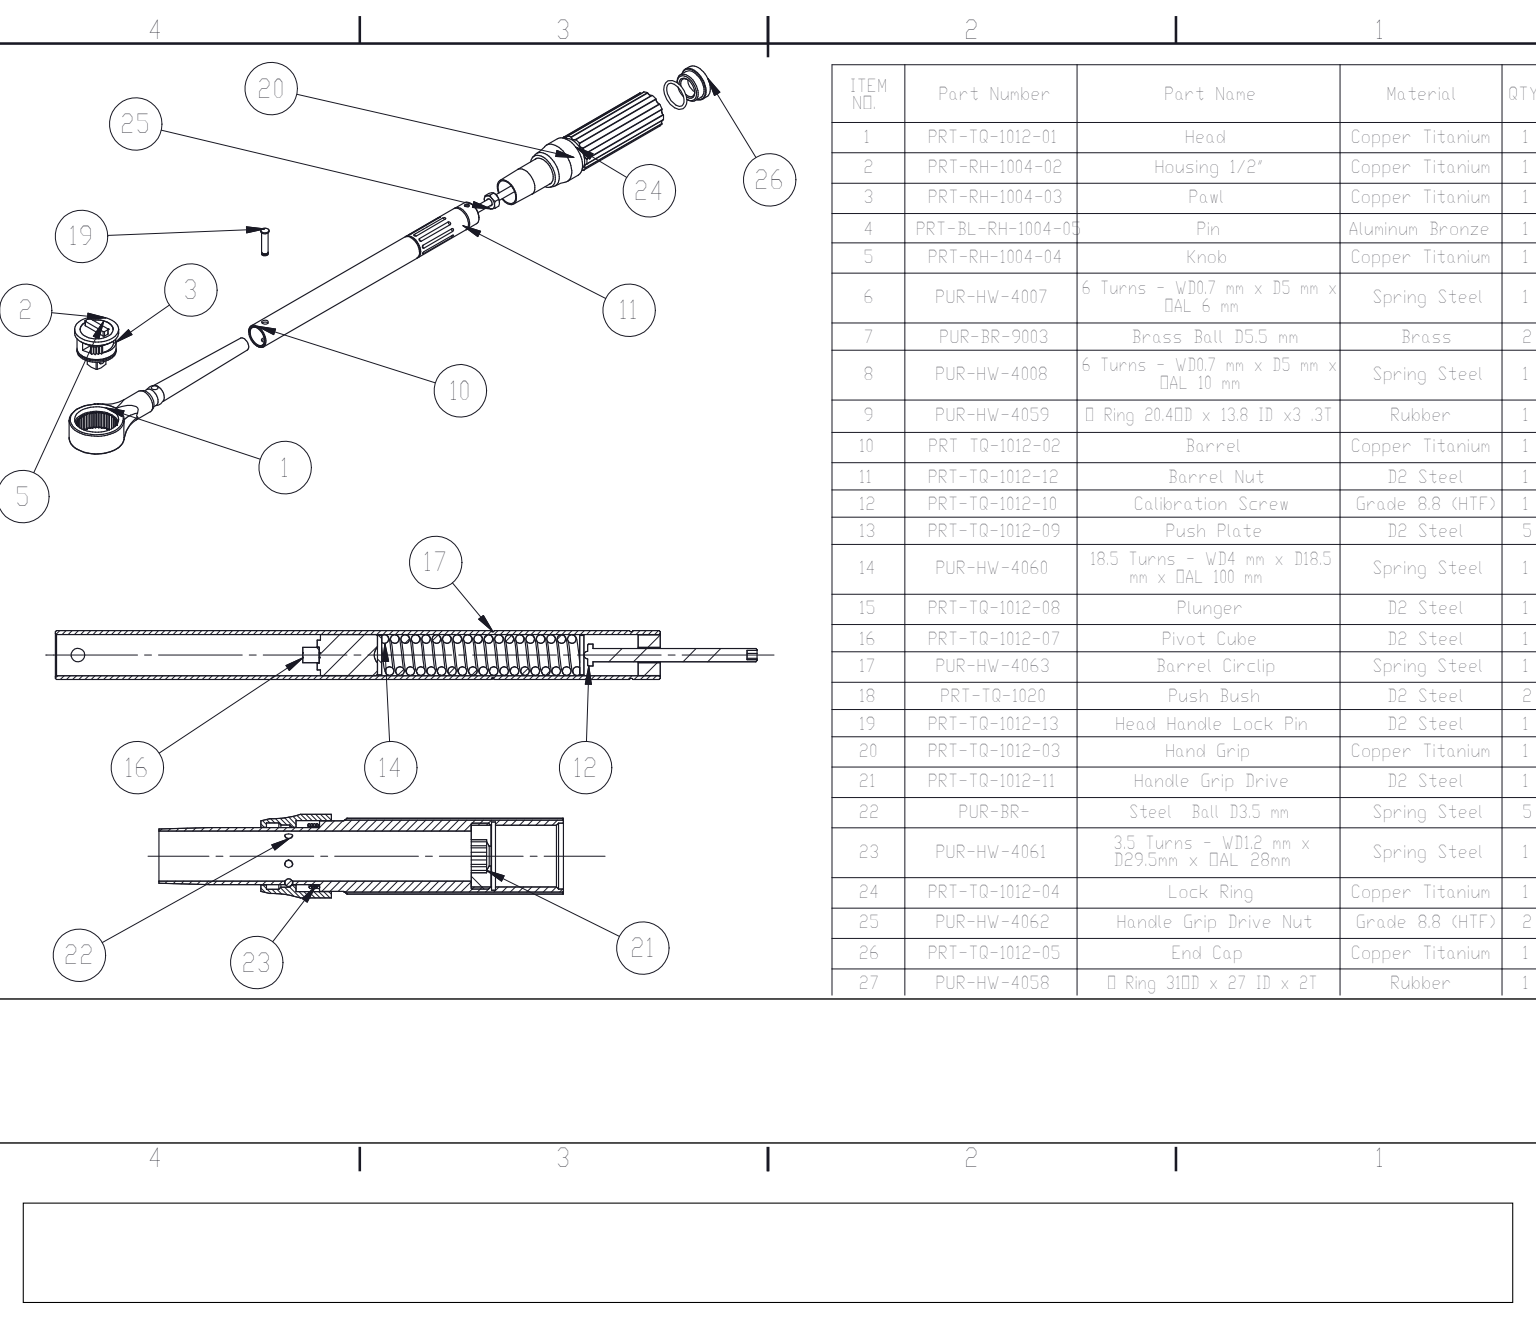
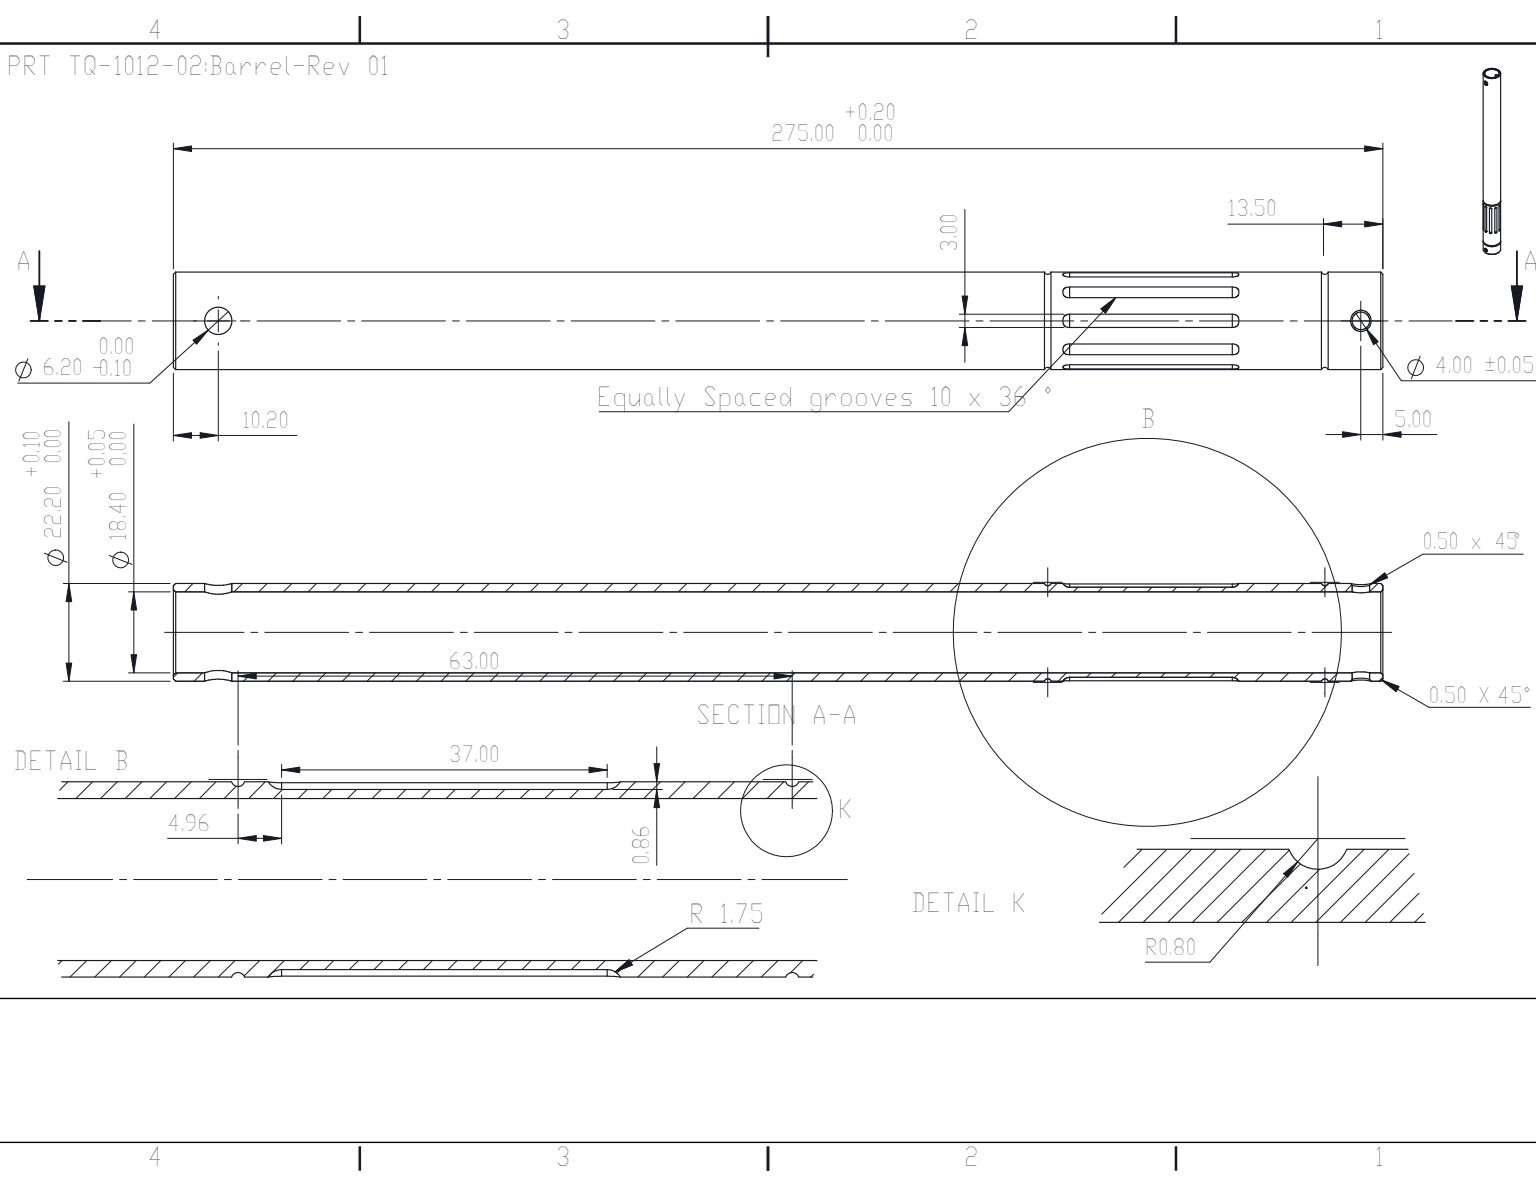
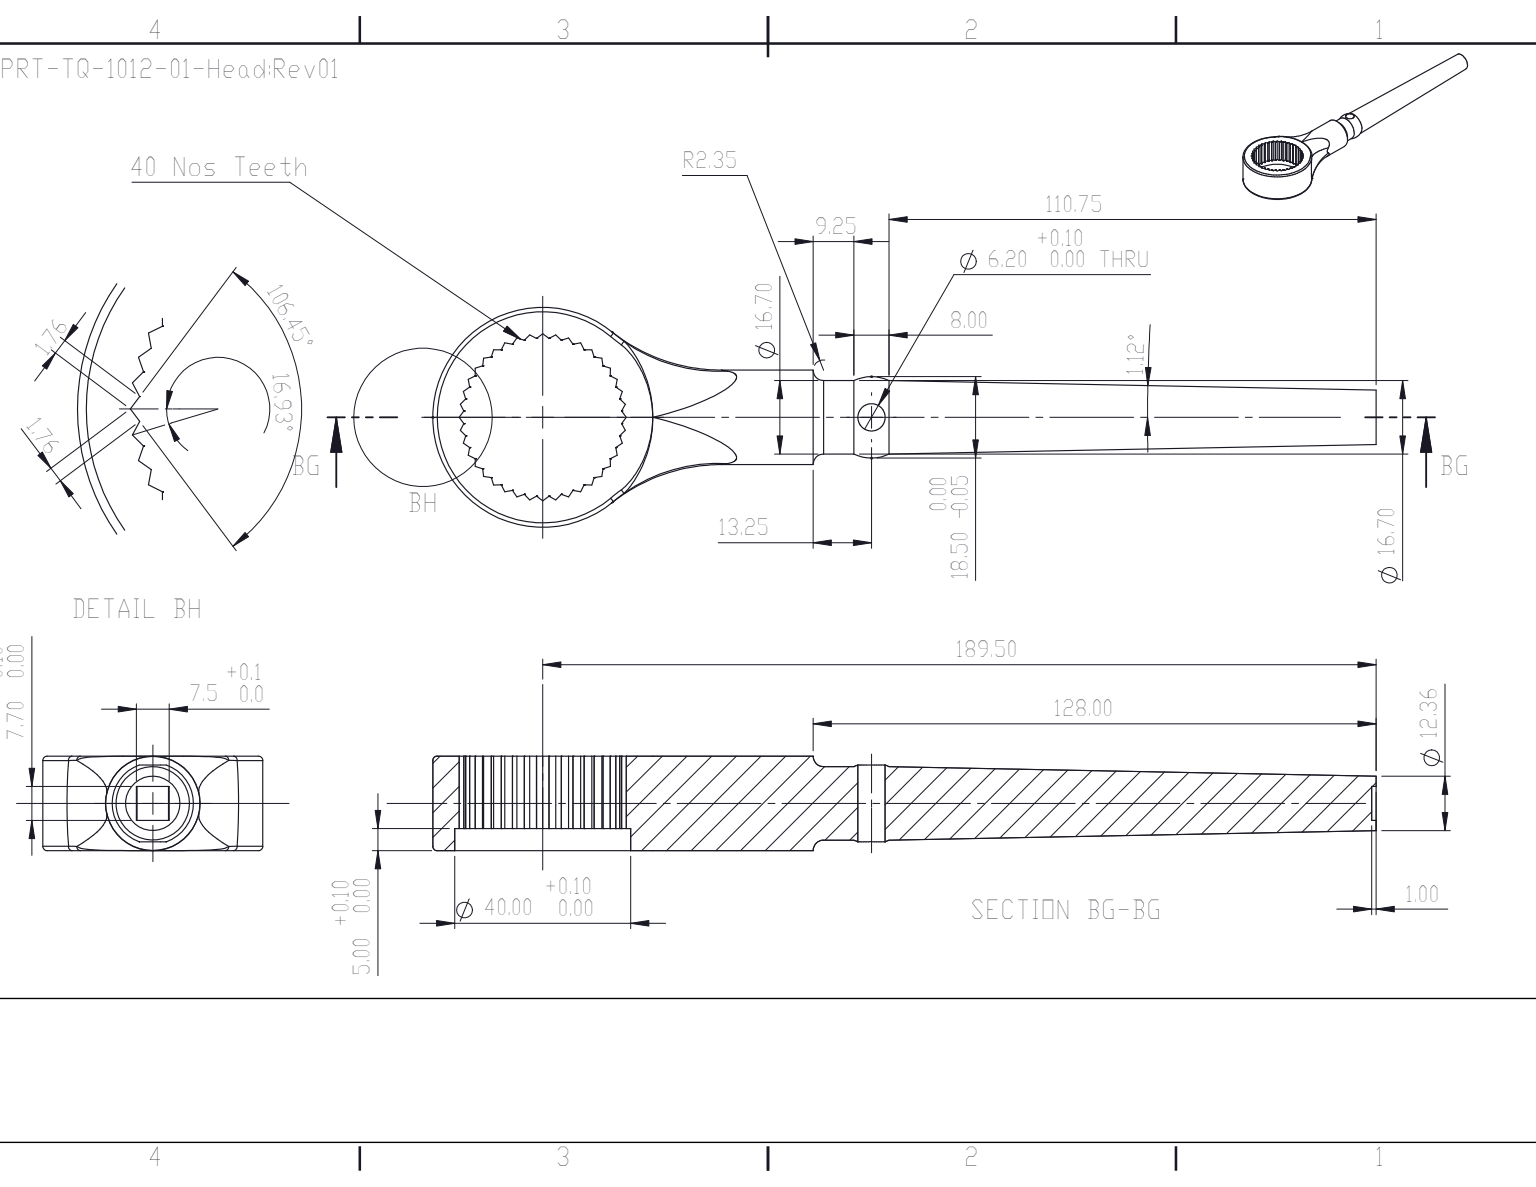
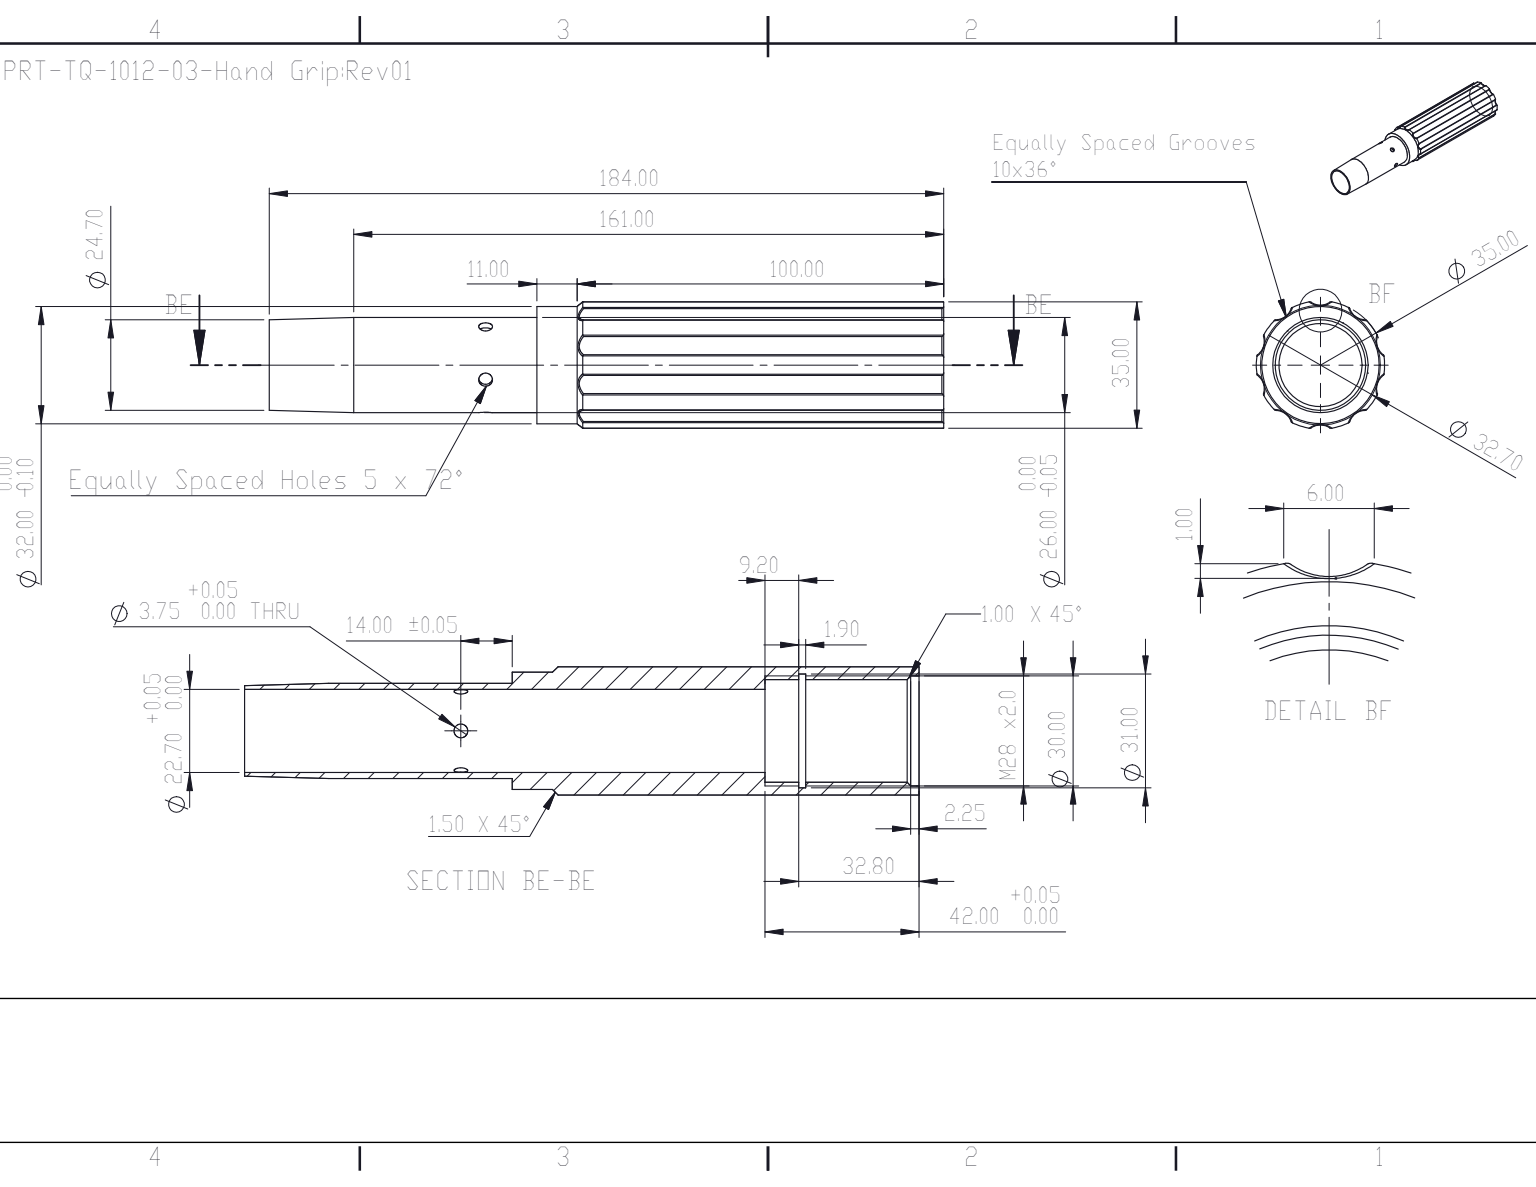
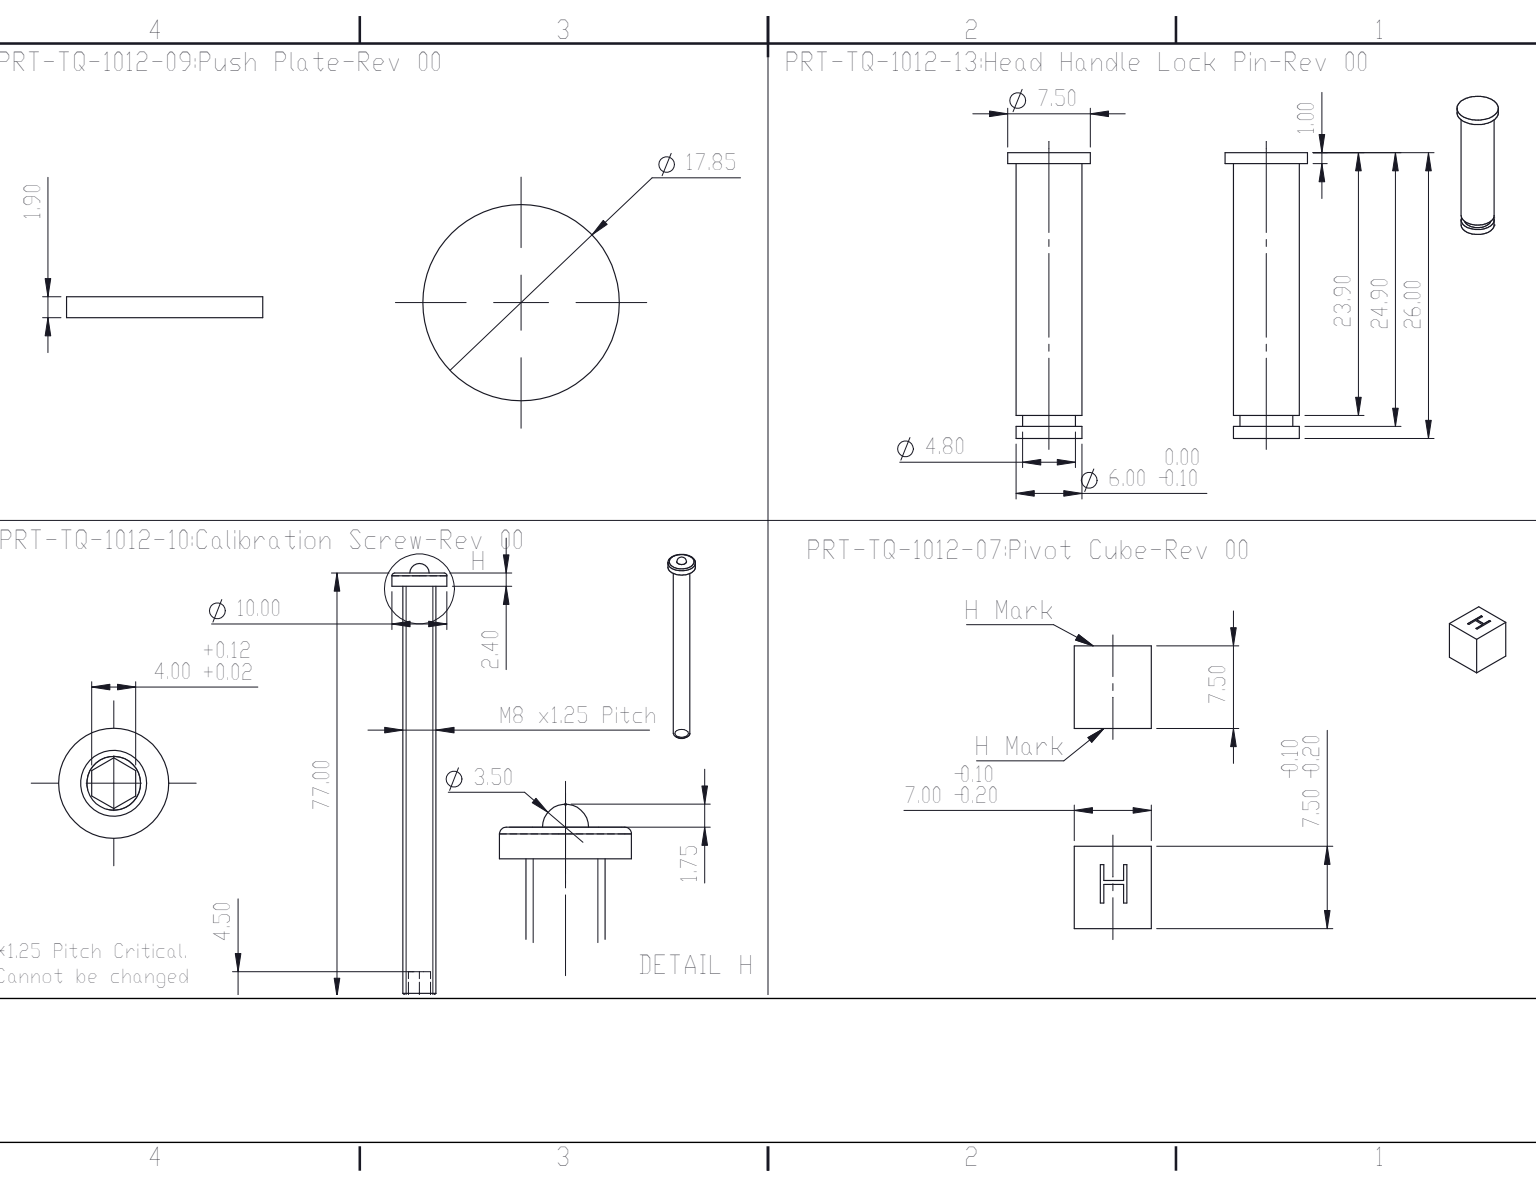
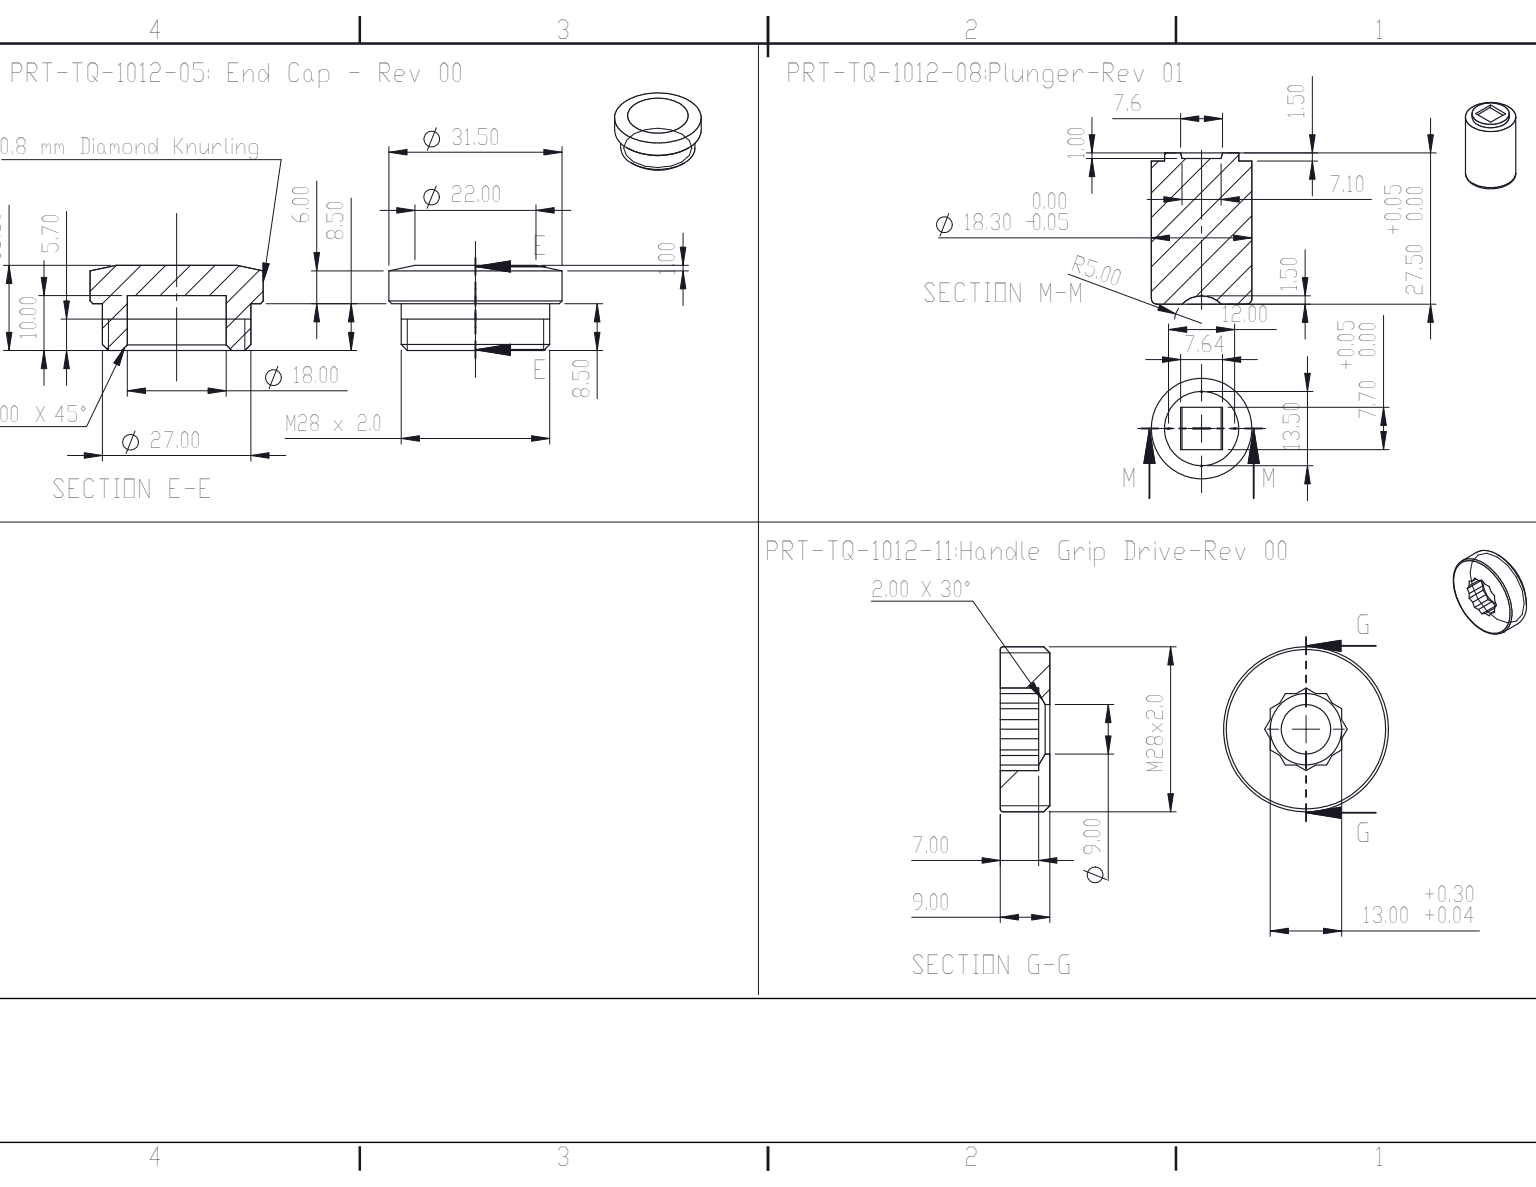
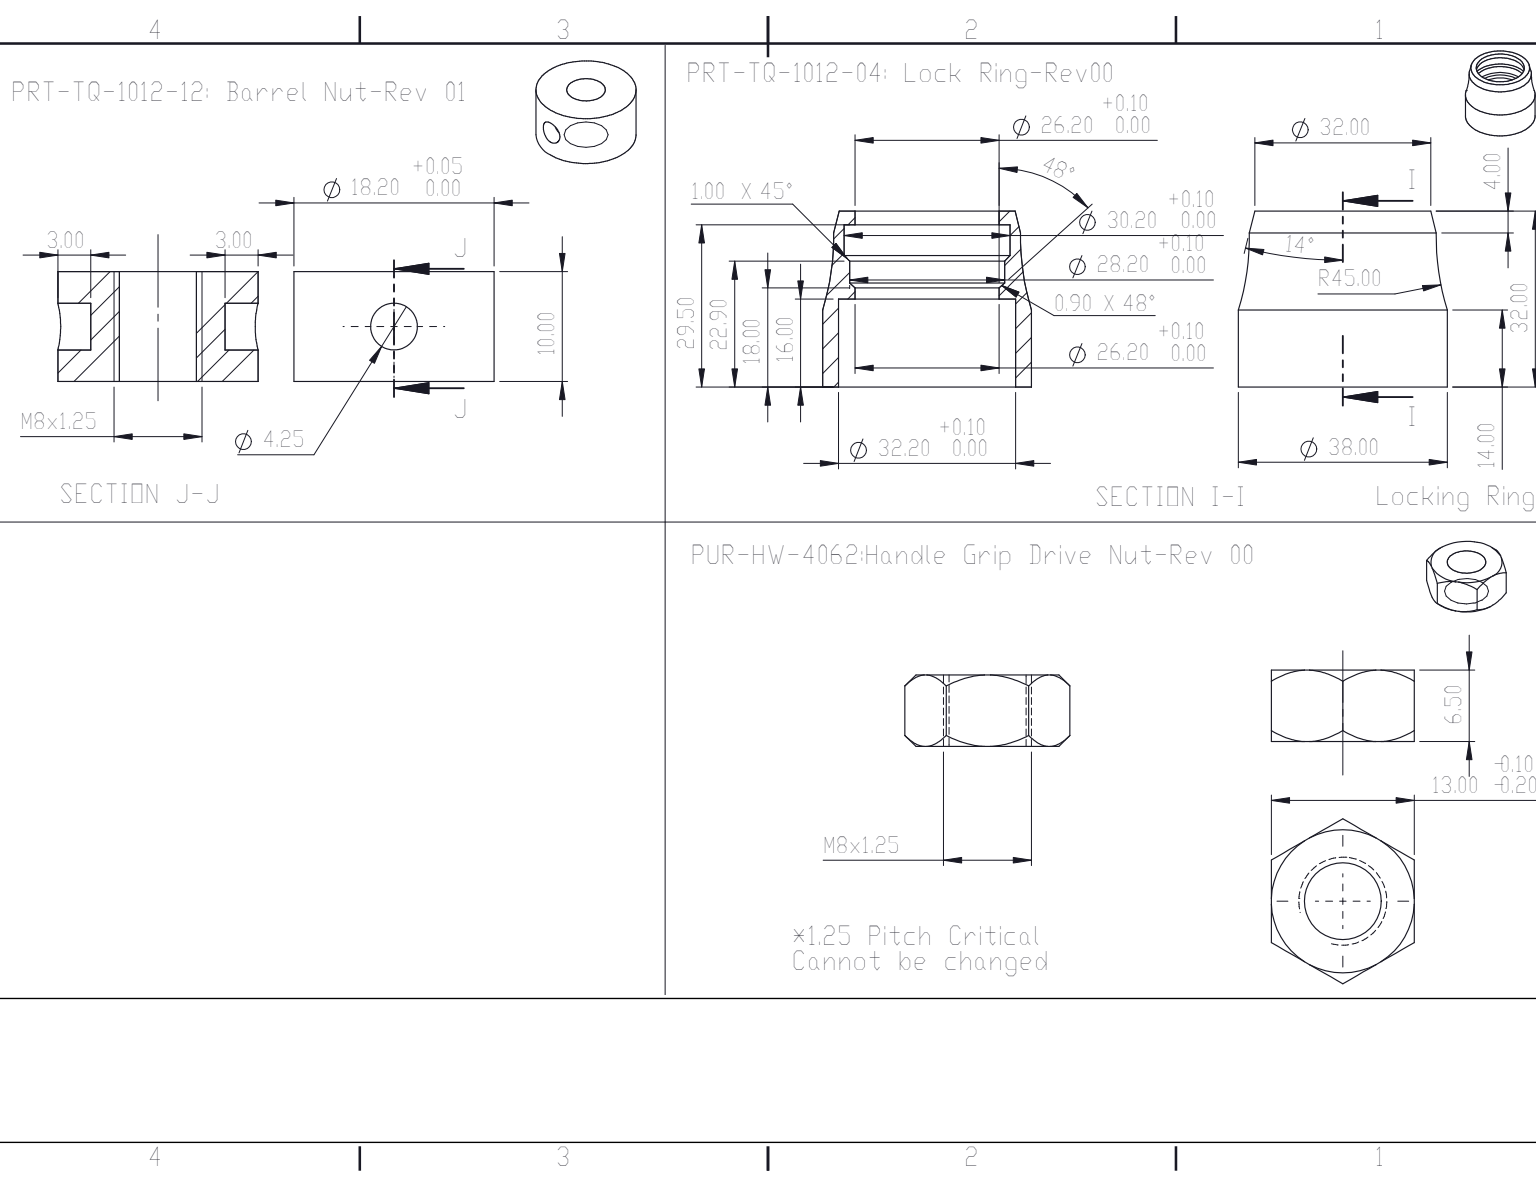
ISO-10303-21;
HEADER;
/* Generated by software containing ST-Developer
 * from STEP Tools, Inc. (www.steptools.com) 
 */

FILE_DESCRIPTION(
/* description */ ('STEP AP214'),
/* implementation_level */ '2;1');

FILE_NAME(
/* name */ 'MAS-618',
/* time_stamp */ '2026-10-07T12:49:37-07:00',
/* author */ (''),
/* organization */ (''),
/* preprocessor_version */ 'ST-DEVELOPER v20.2',
/* originating_system */ 'Autodesk Translation Framework v15.15.0.0',
/* authorisation */ '');

FILE_SCHEMA (('AUTOMOTIVE_DESIGN { 1 0 10303 214 3 1 1 }'));
ENDSEC;

DATA;
#10=MECHANICAL_DESIGN_GEOMETRIC_PRESENTATION_REPRESENTATION('',(#287,#288,
#289,#290,#291,#292,#293,#294,#295,#296,#297,#298,#299,#300,#301,#302,#303,
#304,#305,#306,#307,#308,#309,#310,#311,#312,#313,#314,#315,#316,#317),
#33016);
#11=B_SPLINE_SURFACE_WITH_KNOTS('',1,3,((#22855,#22856,#22857,#22858,#22859,
#22860,#22861,#22862,#22863,#22864,#22865,#22866,#22867,#22868,#22869,#22870,
#22871,#22872,#22873,#22874,#22875,#22876,#22877,#22878,#22879,#22880,#22881,
#22882,#22883,#22884,#22885,#22886,#22887,#22888,#22889,#22890,#22891,#22892,
#22893,#22894,#22895,#22896,#22897,#22898,#22899,#22900,#22901,#22902,#22903,
#22904,#22905,#22906,#22907,#22908,#22909,#22910,#22911,#22912,#22913,#22914,
#22915,#22916,#22917,#22918,#22919,#22920,#22921,#22922,#22923,#22924,#22925,
#22926,#22927,#22928,#22929,#22930,#22931,#22932,#22933,#22934,#22935,#22936,
#22937,#22938,#22939,#22940,#22941,#22942,#22943,#22944,#22945,#22946,#22947,
#22948,#22949,#22950,#22951,#22952,#22953,#22954,#22955,#22956,#22957,#22958,
#22959,#22960,#22961,#22962,#22963,#22964,#22965,#22966,#22967,#22968,#22969,
#22970,#22971,#22972,#22973,#22974,#22975,#22976,#22977,#22978,#22979,#22980,
#22981,#22982,#22983,#22984,#22985,#22986,#22987,#22988,#22989,#22990,#22991,
#22992,#22993,#22994,#22995,#22996,#22997,#22998,#22999,#23000,#23001,#23002,
#23003,#23004,#23005,#23006,#23007,#23008,#23009,#23010,#23011,#23012,#23013,
#23014,#23015,#23016,#23017,#23018,#23019,#23020,#23021,#23022,#23023,#23024,
#23025,#23026,#23027,#23028,#23029,#23030,#23031,#23032,#23033,#23034,#23035,
#23036,#23037,#23038,#23039,#23040,#23041,#23042,#23043,#23044,#23045,#23046,
#23047,#23048,#23049,#23050,#23051,#23052,#23053,#23054,#23055,#23056,#23057,
#23058,#23059,#23060,#23061,#23062,#23063,#23064,#23065,#23066,#23067,#23068,
#23069,#23070,#23071,#23072,#23073,#23074,#23075,#23076,#23077,#23078,#23079,
#23080,#23081,#23082),(#23083,#23084,#23085,#23086,#23087,#23088,#23089,
#23090,#23091,#23092,#23093,#23094,#23095,#23096,#23097,#23098,#23099,#23100,
#23101,#23102,#23103,#23104,#23105,#23106,#23107,#23108,#23109,#23110,#23111,
#23112,#23113,#23114,#23115,#23116,#23117,#23118,#23119,#23120,#23121,#23122,
#23123,#23124,#23125,#23126,#23127,#23128,#23129,#23130,#23131,#23132,#23133,
#23134,#23135,#23136,#23137,#23138,#23139,#23140,#23141,#23142,#23143,#23144,
#23145,#23146,#23147,#23148,#23149,#23150,#23151,#23152,#23153,#23154,#23155,
#23156,#23157,#23158,#23159,#23160,#23161,#23162,#23163,#23164,#23165,#23166,
#23167,#23168,#23169,#23170,#23171,#23172,#23173,#23174,#23175,#23176,#23177,
#23178,#23179,#23180,#23181,#23182,#23183,#23184,#23185,#23186,#23187,#23188,
#23189,#23190,#23191,#23192,#23193,#23194,#23195,#23196,#23197,#23198,#23199,
#23200,#23201,#23202,#23203,#23204,#23205,#23206,#23207,#23208,#23209,#23210,
#23211,#23212,#23213,#23214,#23215,#23216,#23217,#23218,#23219,#23220,#23221,
#23222,#23223,#23224,#23225,#23226,#23227,#23228,#23229,#23230,#23231,#23232,
#23233,#23234,#23235,#23236,#23237,#23238,#23239,#23240,#23241,#23242,#23243,
#23244,#23245,#23246,#23247,#23248,#23249,#23250,#23251,#23252,#23253,#23254,
#23255,#23256,#23257,#23258,#23259,#23260,#23261,#23262,#23263,#23264,#23265,
#23266,#23267,#23268,#23269,#23270,#23271,#23272,#23273,#23274,#23275,#23276,
#23277,#23278,#23279,#23280,#23281,#23282,#23283,#23284,#23285,#23286,#23287,
#23288,#23289,#23290,#23291,#23292,#23293,#23294,#23295,#23296,#23297,#23298,
#23299,#23300,#23301,#23302,#23303,#23304,#23305,#23306,#23307,#23308,#23309,
#23310)),.UNSPECIFIED.,.F.,.T.,.F.,(2,2),(4,2,2,2,2,2,2,2,2,2,2,2,2,2,2,
2,2,2,2,2,2,2,2,2,2,2,2,2,2,2,2,2,2,2,2,2,2,2,2,2,2,2,2,2,2,2,2,2,2,2,2,
2,2,2,2,2,2,2,2,2,2,2,2,2,2,2,2,2,2,2,2,2,2,2,2,2,2,2,2,2,2,2,2,2,2,2,2,
2,2,2,2,2,2,2,2,2,2,2,2,2,2,2,2,2,2,2,2,2,2,2,2,2,2,4),(-3.44305291207021E-6,
1.00001612088686),(0.000602391914111579,0.000716155250734292,0.000829918587357007,
0.000943681923979721,0.00105744526060244,0.00128497193384786,0.00139873527047058,
0.00151249860709329,0.00156938027540465,0.00162626194371601,0.00174002528033872,
0.00196755195358415,0.00208131529020687,0.00219507862682958,0.00230884196345229,
0.00242260530007501,0.00253636863669772,0.00265013197332044,0.00287765864656587,
0.00299142198318858,0.0031051853198113,0.00321894865643401,0.00333271199305672,
0.00356023866630215,0.00378776533954758,0.00384464700785894,0.0039015286761703,
0.00401529201279301,0.00412905534941573,0.00424281868603844,0.00435658202266115,
0.00447034535928387,0.00458410869590658,0.0046978720325293,0.00481163536915201,
0.00492539870577473,0.00515292537902016,0.00526668871564287,0.00538045205226559,
0.00543733372057694,0.0054942153888883,0.00560797872551101,0.00583550539875644,
0.00594926873537916,0.00606303207200187,0.00617679540862459,0.0062905587452473,
0.00651808541849273,0.00674561209173816,0.00697313876498359,0.00720066543822902,
0.00731442877485173,0.00742819211147445,0.00754195544809716,0.00765571878471987,
0.00776948212134259,0.0078832454579653,0.00811077213121073,0.00822453546783345,
0.00833829880445616,0.00845206214107888,0.00856582547770159,0.00879335215094702,
0.00902087882419245,0.00913464216081516,0.00924840549743788,0.00936216883406059,
0.00947593217068331,0.00970345884392873,0.00981722218055145,0.00987410384886281,
0.00993098551717416,0.0100447488537969,0.0101585121904196,0.010386038863665,
0.0104998022002877,0.0106135655369105,0.0107273288735332,0.0108410922101559,
0.0109548555467786,0.0110686188834013,0.011182382220024,0.0112961455566467,
0.0114099088932695,0.0115236722298922,0.0116374355665149,0.0117511989031376,
0.011978725576383,0.0120924889130057,0.0122062522496285,0.0122631339179398,
0.0123200155862512,0.0124337789228739,0.0126613055961193,0.0128888322693647,
0.0130025956059875,0.0131163589426102,0.0132301222792329,0.0133438856158556,
0.013571412289101,0.0136851756257237,0.0137420572940351,0.0137989389623465,
0.0139127022989692,0.0140264656355919,0.0142539923088373,0.0144815189820827,
0.0145384006503941,0.0145952823187055,0.0147090456553282,0.0148228089919509,
0.0149365723285736,0.0150503356651963,0.015164099001819),.UNSPECIFIED.);
#12=B_SPLINE_SURFACE_WITH_KNOTS('',1,3,((#23313,#23314,#23315,#23316,#23317,
#23318,#23319,#23320,#23321,#23322,#23323,#23324,#23325,#23326,#23327,#23328,
#23329,#23330,#23331,#23332,#23333,#23334,#23335,#23336,#23337,#23338,#23339,
#23340,#23341,#23342,#23343,#23344,#23345,#23346,#23347,#23348,#23349,#23350,
#23351,#23352,#23353,#23354,#23355,#23356,#23357,#23358,#23359,#23360,#23361,
#23362,#23363,#23364,#23365,#23366,#23367,#23368,#23369,#23370,#23371,#23372,
#23373,#23374,#23375,#23376,#23377,#23378,#23379,#23380,#23381,#23382,#23383,
#23384,#23385,#23386,#23387,#23388,#23389,#23390,#23391,#23392,#23393,#23394,
#23395,#23396,#23397,#23398,#23399,#23400,#23401,#23402,#23403,#23404,#23405,
#23406,#23407,#23408,#23409,#23410,#23411,#23412,#23413,#23414,#23415,#23416,
#23417,#23418,#23419,#23420,#23421,#23422,#23423,#23424,#23425,#23426,#23427,
#23428,#23429,#23430,#23431,#23432,#23433,#23434,#23435,#23436,#23437,#23438,
#23439,#23440,#23441,#23442,#23443,#23444,#23445,#23446,#23447,#23448,#23449,
#23450,#23451,#23452,#23453,#23454,#23455,#23456,#23457,#23458,#23459,#23460,
#23461,#23462,#23463,#23464,#23465,#23466,#23467,#23468,#23469,#23470,#23471,
#23472,#23473,#23474,#23475,#23476,#23477,#23478,#23479,#23480,#23481,#23482,
#23483,#23484,#23485,#23486,#23487,#23488,#23489,#23490,#23491,#23492,#23493,
#23494,#23495,#23496,#23497,#23498,#23499,#23500,#23501,#23502,#23503,#23504,
#23505,#23506,#23507,#23508,#23509,#23510,#23511,#23512,#23513,#23514,#23515,
#23516,#23517,#23518,#23519,#23520,#23521,#23522,#23523,#23524,#23525,#23526,
#23527,#23528,#23529,#23530,#23531,#23532,#23533,#23534,#23535,#23536,#23537,
#23538),(#23539,#23540,#23541,#23542,#23543,#23544,#23545,#23546,#23547,
#23548,#23549,#23550,#23551,#23552,#23553,#23554,#23555,#23556,#23557,#23558,
#23559,#23560,#23561,#23562,#23563,#23564,#23565,#23566,#23567,#23568,#23569,
#23570,#23571,#23572,#23573,#23574,#23575,#23576,#23577,#23578,#23579,#23580,
#23581,#23582,#23583,#23584,#23585,#23586,#23587,#23588,#23589,#23590,#23591,
#23592,#23593,#23594,#23595,#23596,#23597,#23598,#23599,#23600,#23601,#23602,
#23603,#23604,#23605,#23606,#23607,#23608,#23609,#23610,#23611,#23612,#23613,
#23614,#23615,#23616,#23617,#23618,#23619,#23620,#23621,#23622,#23623,#23624,
#23625,#23626,#23627,#23628,#23629,#23630,#23631,#23632,#23633,#23634,#23635,
#23636,#23637,#23638,#23639,#23640,#23641,#23642,#23643,#23644,#23645,#23646,
#23647,#23648,#23649,#23650,#23651,#23652,#23653,#23654,#23655,#23656,#23657,
#23658,#23659,#23660,#23661,#23662,#23663,#23664,#23665,#23666,#23667,#23668,
#23669,#23670,#23671,#23672,#23673,#23674,#23675,#23676,#23677,#23678,#23679,
#23680,#23681,#23682,#23683,#23684,#23685,#23686,#23687,#23688,#23689,#23690,
#23691,#23692,#23693,#23694,#23695,#23696,#23697,#23698,#23699,#23700,#23701,
#23702,#23703,#23704,#23705,#23706,#23707,#23708,#23709,#23710,#23711,#23712,
#23713,#23714,#23715,#23716,#23717,#23718,#23719,#23720,#23721,#23722,#23723,
#23724,#23725,#23726,#23727,#23728,#23729,#23730,#23731,#23732,#23733,#23734,
#23735,#23736,#23737,#23738,#23739,#23740,#23741,#23742,#23743,#23744,#23745,
#23746,#23747,#23748,#23749,#23750,#23751,#23752,#23753,#23754,#23755,#23756,
#23757,#23758,#23759,#23760,#23761,#23762,#23763,#23764)),.UNSPECIFIED.,
 .F.,.T.,.F.,(2,2),(4,2,2,2,2,2,2,2,2,2,2,2,2,2,2,2,2,2,2,2,2,2,2,2,2,2,
2,2,2,2,2,2,2,2,2,2,2,2,2,2,2,2,2,2,2,2,2,2,2,2,2,2,2,2,2,2,2,2,2,2,2,2,
2,2,2,2,2,2,2,2,2,2,2,2,2,2,2,2,2,2,2,2,2,2,2,2,2,2,2,2,2,2,2,2,2,2,2,2,
2,2,2,2,2,2,2,2,2,2,2,2,2,2,4),(-7.24489232955387E-6,1.00002207748051),
(0.000580381745839097,0.000694149846669441,0.000751033897084613,0.000807917947499785,
0.00092168604833013,0.00103545414916048,0.00126299035082116,0.00137675845165151,
0.00149052655248185,0.0016042946533122,0.00171806275414254,0.00183183085497289,
0.00194559895580323,0.00205936705663358,0.00217313515746392,0.00228690325829427,
0.00234378730870944,0.00240067135912461,0.0026282075607853,0.00285574376244599,
0.00296951186327634,0.00308327996410668,0.00319704806493703,0.00331081616576737,
0.00353835236742806,0.00365212046825841,0.00376588856908875,0.00387965666991909,
0.00399342477074944,0.00410719287157978,0.00422096097241013,0.00444849717407082,
0.00456226527490116,0.00461914932531634,0.00467603337573151,0.00478980147656185,
0.0049035695773922,0.00513110577905289,0.00524487387988323,0.00535864198071358,
0.00547241008154392,0.00558617818237427,0.00569994628320461,0.00581371438403496,
0.0059274824848653,0.00604125058569565,0.00615501868652599,0.00621190273694116,
0.00626878678735633,0.00649632298901703,0.00672385919067771,0.00683762729150806,
0.0069513953923384,0.00706516349316875,0.00717893159399909,0.00740646779565978,
0.00752023589649013,0.00763400399732047,0.00774777209815082,0.00786154019898116,
0.00808907640064185,0.00820284450147219,0.00831661260230254,0.00837349665271771,
0.00843038070313289,0.00854414880396323,0.00877168500562392,0.00888545310645426,
0.00899922120728461,0.00911298930811495,0.0092267574089453,0.00934052550977564,
0.00945429361060599,0.00968182981226668,0.00979559791309702,0.00990936601392737,
0.0100231341147577,0.0101369022155881,0.0103644384172487,0.0105919746189094,
0.0106488586693246,0.0107057427197398,0.0108195108205701,0.0109332789214005,
0.0110470470222308,0.0112745832238915,0.0113883513247218,0.011445235375137,
0.0115021194255522,0.0116158875263825,0.0117296556272129,0.0119571918288736,
0.0120709599297039,0.0121847280305343,0.0122984961313646,0.012412264232195,
0.0125260323330253,0.0126398004338556,0.012753568534686,0.0128673366355163,
0.0129811047363467,0.013094872837177,0.0133224090388377,0.0135499452404984,
0.0137774814421591,0.0140050176438198,0.0142325538454805,0.0144600900471412,
0.0145738581479715,0.0146876262488018,0.0148013943496322,0.0149151624504625,
0.0151426986521232),.UNSPECIFIED.);
#13=ITEM_DEFINED_TRANSFORMATION($,$,#10519,#10691);
#14=ITEM_DEFINED_TRANSFORMATION($,$,#10580,#10692);
#15=ITEM_DEFINED_TRANSFORMATION($,$,#10615,#10693);
#16=ITEM_DEFINED_TRANSFORMATION($,$,#10626,#10694);
#17=ITEM_DEFINED_TRANSFORMATION($,$,#10666,#10695);
#18=ITEM_DEFINED_TRANSFORMATION($,$,#10688,#10696);
#19=ITEM_DEFINED_TRANSFORMATION($,$,#10677,#10697);
#20=ITEM_DEFINED_TRANSFORMATION($,$,#10688,#10698);
#21=ITEM_DEFINED_TRANSFORMATION($,$,#10704,#10890);
#22=ITEM_DEFINED_TRANSFORMATION($,$,#10767,#10891);
#23=ITEM_DEFINED_TRANSFORMATION($,$,#10782,#10892);
#24=ITEM_DEFINED_TRANSFORMATION($,$,#10875,#10893);
#25=ITEM_DEFINED_TRANSFORMATION($,$,#10807,#10894);
#26=ITEM_DEFINED_TRANSFORMATION($,$,#10814,#10895);
#27=ITEM_DEFINED_TRANSFORMATION($,$,#10835,#10896);
#28=ITEM_DEFINED_TRANSFORMATION($,$,#10868,#10897);
#29=ITEM_DEFINED_TRANSFORMATION($,$,#10881,#10898);
#30=ITEM_DEFINED_TRANSFORMATION($,$,#10875,#10899);
#31=ITEM_DEFINED_TRANSFORMATION($,$,#10875,#10900);
#32=ITEM_DEFINED_TRANSFORMATION($,$,#10875,#10901);
#33=ITEM_DEFINED_TRANSFORMATION($,$,#10875,#10902);
#34=ITEM_DEFINED_TRANSFORMATION($,$,#10881,#10903);
#35=ITEM_DEFINED_TRANSFORMATION($,$,#10923,#11150);
#36=ITEM_DEFINED_TRANSFORMATION($,$,#11059,#11151);
#37=ITEM_DEFINED_TRANSFORMATION($,$,#11147,#11152);
#38=ITEM_DEFINED_TRANSFORMATION($,$,#11102,#11153);
#39=ITEM_DEFINED_TRANSFORMATION($,$,#11113,#11154);
#40=ITEM_DEFINED_TRANSFORMATION($,$,#11147,#11155);
#41=ITEM_DEFINED_TRANSFORMATION($,$,#11147,#11156);
#42=ITEM_DEFINED_TRANSFORMATION($,$,#11147,#11157);
#43=ITEM_DEFINED_TRANSFORMATION($,$,#11147,#11158);
#44=ITEM_DEFINED_TRANSFORMATION($,$,#10268,#11223);
#45=ITEM_DEFINED_TRANSFORMATION($,$,#10518,#11224);
#46=ITEM_DEFINED_TRANSFORMATION($,$,#10699,#11225);
#47=ITEM_DEFINED_TRANSFORMATION($,$,#10703,#11226);
#48=ITEM_DEFINED_TRANSFORMATION($,$,#10904,#11227);
#49=ITEM_DEFINED_TRANSFORMATION($,$,#10922,#11228);
#50=ITEM_DEFINED_TRANSFORMATION($,$,#11187,#11229);
#51=ITEM_DEFINED_TRANSFORMATION($,$,#11159,#11230);
#52=ITEM_DEFINED_TRANSFORMATION($,$,#11183,#11231);
#53=ITEM_DEFINED_TRANSFORMATION($,$,#11187,#11232);
#54=(
REPRESENTATION_RELATIONSHIP($,$,#33127,#33126)
REPRESENTATION_RELATIONSHIP_WITH_TRANSFORMATION(#13)
SHAPE_REPRESENTATION_RELATIONSHIP()
);
#55=(
REPRESENTATION_RELATIONSHIP($,$,#33128,#33126)
REPRESENTATION_RELATIONSHIP_WITH_TRANSFORMATION(#14)
SHAPE_REPRESENTATION_RELATIONSHIP()
);
#56=(
REPRESENTATION_RELATIONSHIP($,$,#33129,#33126)
REPRESENTATION_RELATIONSHIP_WITH_TRANSFORMATION(#15)
SHAPE_REPRESENTATION_RELATIONSHIP()
);
#57=(
REPRESENTATION_RELATIONSHIP($,$,#33130,#33126)
REPRESENTATION_RELATIONSHIP_WITH_TRANSFORMATION(#16)
SHAPE_REPRESENTATION_RELATIONSHIP()
);
#58=(
REPRESENTATION_RELATIONSHIP($,$,#33131,#33126)
REPRESENTATION_RELATIONSHIP_WITH_TRANSFORMATION(#17)
SHAPE_REPRESENTATION_RELATIONSHIP()
);
#59=(
REPRESENTATION_RELATIONSHIP($,$,#33133,#33126)
REPRESENTATION_RELATIONSHIP_WITH_TRANSFORMATION(#18)
SHAPE_REPRESENTATION_RELATIONSHIP()
);
#60=(
REPRESENTATION_RELATIONSHIP($,$,#33132,#33126)
REPRESENTATION_RELATIONSHIP_WITH_TRANSFORMATION(#19)
SHAPE_REPRESENTATION_RELATIONSHIP()
);
#61=(
REPRESENTATION_RELATIONSHIP($,$,#33133,#33126)
REPRESENTATION_RELATIONSHIP_WITH_TRANSFORMATION(#20)
SHAPE_REPRESENTATION_RELATIONSHIP()
);
#62=(
REPRESENTATION_RELATIONSHIP($,$,#33136,#33135)
REPRESENTATION_RELATIONSHIP_WITH_TRANSFORMATION(#21)
SHAPE_REPRESENTATION_RELATIONSHIP()
);
#63=(
REPRESENTATION_RELATIONSHIP($,$,#33137,#33135)
REPRESENTATION_RELATIONSHIP_WITH_TRANSFORMATION(#22)
SHAPE_REPRESENTATION_RELATIONSHIP()
);
#64=(
REPRESENTATION_RELATIONSHIP($,$,#33138,#33135)
REPRESENTATION_RELATIONSHIP_WITH_TRANSFORMATION(#23)
SHAPE_REPRESENTATION_RELATIONSHIP()
);
#65=(
REPRESENTATION_RELATIONSHIP($,$,#33143,#33135)
REPRESENTATION_RELATIONSHIP_WITH_TRANSFORMATION(#24)
SHAPE_REPRESENTATION_RELATIONSHIP()
);
#66=(
REPRESENTATION_RELATIONSHIP($,$,#33139,#33135)
REPRESENTATION_RELATIONSHIP_WITH_TRANSFORMATION(#25)
SHAPE_REPRESENTATION_RELATIONSHIP()
);
#67=(
REPRESENTATION_RELATIONSHIP($,$,#33140,#33135)
REPRESENTATION_RELATIONSHIP_WITH_TRANSFORMATION(#26)
SHAPE_REPRESENTATION_RELATIONSHIP()
);
#68=(
REPRESENTATION_RELATIONSHIP($,$,#33141,#33135)
REPRESENTATION_RELATIONSHIP_WITH_TRANSFORMATION(#27)
SHAPE_REPRESENTATION_RELATIONSHIP()
);
#69=(
REPRESENTATION_RELATIONSHIP($,$,#33142,#33135)
REPRESENTATION_RELATIONSHIP_WITH_TRANSFORMATION(#28)
SHAPE_REPRESENTATION_RELATIONSHIP()
);
#70=(
REPRESENTATION_RELATIONSHIP($,$,#33144,#33135)
REPRESENTATION_RELATIONSHIP_WITH_TRANSFORMATION(#29)
SHAPE_REPRESENTATION_RELATIONSHIP()
);
#71=(
REPRESENTATION_RELATIONSHIP($,$,#33143,#33135)
REPRESENTATION_RELATIONSHIP_WITH_TRANSFORMATION(#30)
SHAPE_REPRESENTATION_RELATIONSHIP()
);
#72=(
REPRESENTATION_RELATIONSHIP($,$,#33143,#33135)
REPRESENTATION_RELATIONSHIP_WITH_TRANSFORMATION(#31)
SHAPE_REPRESENTATION_RELATIONSHIP()
);
#73=(
REPRESENTATION_RELATIONSHIP($,$,#33143,#33135)
REPRESENTATION_RELATIONSHIP_WITH_TRANSFORMATION(#32)
SHAPE_REPRESENTATION_RELATIONSHIP()
);
#74=(
REPRESENTATION_RELATIONSHIP($,$,#33143,#33135)
REPRESENTATION_RELATIONSHIP_WITH_TRANSFORMATION(#33)
SHAPE_REPRESENTATION_RELATIONSHIP()
);
#75=(
REPRESENTATION_RELATIONSHIP($,$,#33144,#33135)
REPRESENTATION_RELATIONSHIP_WITH_TRANSFORMATION(#34)
SHAPE_REPRESENTATION_RELATIONSHIP()
);
#76=(
REPRESENTATION_RELATIONSHIP($,$,#33147,#33146)
REPRESENTATION_RELATIONSHIP_WITH_TRANSFORMATION(#35)
SHAPE_REPRESENTATION_RELATIONSHIP()
);
#77=(
REPRESENTATION_RELATIONSHIP($,$,#33148,#33146)
REPRESENTATION_RELATIONSHIP_WITH_TRANSFORMATION(#36)
SHAPE_REPRESENTATION_RELATIONSHIP()
);
#78=(
REPRESENTATION_RELATIONSHIP($,$,#33151,#33146)
REPRESENTATION_RELATIONSHIP_WITH_TRANSFORMATION(#37)
SHAPE_REPRESENTATION_RELATIONSHIP()
);
#79=(
REPRESENTATION_RELATIONSHIP($,$,#33149,#33146)
REPRESENTATION_RELATIONSHIP_WITH_TRANSFORMATION(#38)
SHAPE_REPRESENTATION_RELATIONSHIP()
);
#80=(
REPRESENTATION_RELATIONSHIP($,$,#33150,#33146)
REPRESENTATION_RELATIONSHIP_WITH_TRANSFORMATION(#39)
SHAPE_REPRESENTATION_RELATIONSHIP()
);
#81=(
REPRESENTATION_RELATIONSHIP($,$,#33151,#33146)
REPRESENTATION_RELATIONSHIP_WITH_TRANSFORMATION(#40)
SHAPE_REPRESENTATION_RELATIONSHIP()
);
#82=(
REPRESENTATION_RELATIONSHIP($,$,#33151,#33146)
REPRESENTATION_RELATIONSHIP_WITH_TRANSFORMATION(#41)
SHAPE_REPRESENTATION_RELATIONSHIP()
);
#83=(
REPRESENTATION_RELATIONSHIP($,$,#33151,#33146)
REPRESENTATION_RELATIONSHIP_WITH_TRANSFORMATION(#42)
SHAPE_REPRESENTATION_RELATIONSHIP()
);
#84=(
REPRESENTATION_RELATIONSHIP($,$,#33151,#33146)
REPRESENTATION_RELATIONSHIP_WITH_TRANSFORMATION(#43)
SHAPE_REPRESENTATION_RELATIONSHIP()
);
#85=(
REPRESENTATION_RELATIONSHIP($,$,#33125,#33124)
REPRESENTATION_RELATIONSHIP_WITH_TRANSFORMATION(#44)
SHAPE_REPRESENTATION_RELATIONSHIP()
);
#86=(
REPRESENTATION_RELATIONSHIP($,$,#33126,#33124)
REPRESENTATION_RELATIONSHIP_WITH_TRANSFORMATION(#45)
SHAPE_REPRESENTATION_RELATIONSHIP()
);
#87=(
REPRESENTATION_RELATIONSHIP($,$,#33134,#33124)
REPRESENTATION_RELATIONSHIP_WITH_TRANSFORMATION(#46)
SHAPE_REPRESENTATION_RELATIONSHIP()
);
#88=(
REPRESENTATION_RELATIONSHIP($,$,#33135,#33124)
REPRESENTATION_RELATIONSHIP_WITH_TRANSFORMATION(#47)
SHAPE_REPRESENTATION_RELATIONSHIP()
);
#89=(
REPRESENTATION_RELATIONSHIP($,$,#33145,#33124)
REPRESENTATION_RELATIONSHIP_WITH_TRANSFORMATION(#48)
SHAPE_REPRESENTATION_RELATIONSHIP()
);
#90=(
REPRESENTATION_RELATIONSHIP($,$,#33146,#33124)
REPRESENTATION_RELATIONSHIP_WITH_TRANSFORMATION(#49)
SHAPE_REPRESENTATION_RELATIONSHIP()
);
#91=(
REPRESENTATION_RELATIONSHIP($,$,#33154,#33124)
REPRESENTATION_RELATIONSHIP_WITH_TRANSFORMATION(#50)
SHAPE_REPRESENTATION_RELATIONSHIP()
);
#92=(
REPRESENTATION_RELATIONSHIP($,$,#33152,#33124)
REPRESENTATION_RELATIONSHIP_WITH_TRANSFORMATION(#51)
SHAPE_REPRESENTATION_RELATIONSHIP()
);
#93=(
REPRESENTATION_RELATIONSHIP($,$,#33153,#33124)
REPRESENTATION_RELATIONSHIP_WITH_TRANSFORMATION(#52)
SHAPE_REPRESENTATION_RELATIONSHIP()
);
#94=(
REPRESENTATION_RELATIONSHIP($,$,#33154,#33124)
REPRESENTATION_RELATIONSHIP_WITH_TRANSFORMATION(#53)
SHAPE_REPRESENTATION_RELATIONSHIP()
);
#95=CONTEXT_DEPENDENT_SHAPE_REPRESENTATION(#54,#33062);
#96=CONTEXT_DEPENDENT_SHAPE_REPRESENTATION(#55,#33063);
#97=CONTEXT_DEPENDENT_SHAPE_REPRESENTATION(#56,#33064);
#98=CONTEXT_DEPENDENT_SHAPE_REPRESENTATION(#57,#33065);
#99=CONTEXT_DEPENDENT_SHAPE_REPRESENTATION(#58,#33066);
#100=CONTEXT_DEPENDENT_SHAPE_REPRESENTATION(#59,#33067);
#101=CONTEXT_DEPENDENT_SHAPE_REPRESENTATION(#60,#33068);
#102=CONTEXT_DEPENDENT_SHAPE_REPRESENTATION(#61,#33069);
#103=CONTEXT_DEPENDENT_SHAPE_REPRESENTATION(#62,#33081);
#104=CONTEXT_DEPENDENT_SHAPE_REPRESENTATION(#63,#33082);
#105=CONTEXT_DEPENDENT_SHAPE_REPRESENTATION(#64,#33083);
#106=CONTEXT_DEPENDENT_SHAPE_REPRESENTATION(#65,#33084);
#107=CONTEXT_DEPENDENT_SHAPE_REPRESENTATION(#66,#33085);
#108=CONTEXT_DEPENDENT_SHAPE_REPRESENTATION(#67,#33086);
#109=CONTEXT_DEPENDENT_SHAPE_REPRESENTATION(#68,#33087);
#110=CONTEXT_DEPENDENT_SHAPE_REPRESENTATION(#69,#33088);
#111=CONTEXT_DEPENDENT_SHAPE_REPRESENTATION(#70,#33089);
#112=CONTEXT_DEPENDENT_SHAPE_REPRESENTATION(#71,#33090);
#113=CONTEXT_DEPENDENT_SHAPE_REPRESENTATION(#72,#33091);
#114=CONTEXT_DEPENDENT_SHAPE_REPRESENTATION(#73,#33092);
#115=CONTEXT_DEPENDENT_SHAPE_REPRESENTATION(#74,#33093);
#116=CONTEXT_DEPENDENT_SHAPE_REPRESENTATION(#75,#33094);
#117=CONTEXT_DEPENDENT_SHAPE_REPRESENTATION(#76,#33102);
#118=CONTEXT_DEPENDENT_SHAPE_REPRESENTATION(#77,#33103);
#119=CONTEXT_DEPENDENT_SHAPE_REPRESENTATION(#78,#33104);
#120=CONTEXT_DEPENDENT_SHAPE_REPRESENTATION(#79,#33105);
#121=CONTEXT_DEPENDENT_SHAPE_REPRESENTATION(#80,#33106);
#122=CONTEXT_DEPENDENT_SHAPE_REPRESENTATION(#81,#33107);
#123=CONTEXT_DEPENDENT_SHAPE_REPRESENTATION(#82,#33108);
#124=CONTEXT_DEPENDENT_SHAPE_REPRESENTATION(#83,#33109);
#125=CONTEXT_DEPENDENT_SHAPE_REPRESENTATION(#84,#33110);
#126=CONTEXT_DEPENDENT_SHAPE_REPRESENTATION(#85,#33114);
#127=CONTEXT_DEPENDENT_SHAPE_REPRESENTATION(#86,#33115);
#128=CONTEXT_DEPENDENT_SHAPE_REPRESENTATION(#87,#33116);
#129=CONTEXT_DEPENDENT_SHAPE_REPRESENTATION(#88,#33117);
#130=CONTEXT_DEPENDENT_SHAPE_REPRESENTATION(#89,#33118);
#131=CONTEXT_DEPENDENT_SHAPE_REPRESENTATION(#90,#33119);
#132=CONTEXT_DEPENDENT_SHAPE_REPRESENTATION(#91,#33120);
#133=CONTEXT_DEPENDENT_SHAPE_REPRESENTATION(#92,#33121);
#134=CONTEXT_DEPENDENT_SHAPE_REPRESENTATION(#93,#33122);
#135=CONTEXT_DEPENDENT_SHAPE_REPRESENTATION(#94,#33123);
#136=NEXT_ASSEMBLY_USAGE_OCCURRENCE('PRT-RH-1004-02:1',
'PRT-RH-1004-02:1','PRT-RH-1004-02:1',#33158,#33159,'PRT-RH-1004-02:1');
#137=NEXT_ASSEMBLY_USAGE_OCCURRENCE('PRT-RH-1004-03:1',
'PRT-RH-1004-03:1','PRT-RH-1004-03:1',#33158,#33160,'PRT-RH-1004-03:1');
#138=NEXT_ASSEMBLY_USAGE_OCCURRENCE('PRT-BL-RH-1004-05:1',
'PRT-BL-RH-1004-05:1','PRT-BL-RH-1004-05:1',#33158,#33161,
'PRT-BL-RH-1004-05:1');
#139=NEXT_ASSEMBLY_USAGE_OCCURRENCE('PRT-RH-1004-04:1',
'PRT-RH-1004-04:1','PRT-RH-1004-04:1',#33158,#33162,'PRT-RH-1004-04:1');
#140=NEXT_ASSEMBLY_USAGE_OCCURRENCE('PUR-HW-4007:1','PUR-HW-4007:1',
'PUR-HW-4007:1',#33158,#33163,'PUR-HW-4007:1');
#141=NEXT_ASSEMBLY_USAGE_OCCURRENCE('PUR-BR-9003:1','PUR-BR-9003:1',
'PUR-BR-9003:1',#33158,#33165,'PUR-BR-9003:1');
#142=NEXT_ASSEMBLY_USAGE_OCCURRENCE('PUR-HW-4008:1','PUR-HW-4008:1',
'PUR-HW-4008:1',#33158,#33164,'PUR-HW-4008:1');
#143=NEXT_ASSEMBLY_USAGE_OCCURRENCE('PUR-BR-9003:2','PUR-BR-9003:2',
'PUR-BR-9003:2',#33158,#33165,'PUR-BR-9003:2');
#144=NEXT_ASSEMBLY_USAGE_OCCURRENCE('PRT-TQ-1012-02:1',
'PRT-TQ-1012-02:1','PRT-TQ-1012-02:1',#33167,#33168,'PRT-TQ-1012-02:1');
#145=NEXT_ASSEMBLY_USAGE_OCCURRENCE('PRT-TQ-1012-12:1',
'PRT-TQ-1012-12:1','PRT-TQ-1012-12:1',#33167,#33169,'PRT-TQ-1012-12:1');
#146=NEXT_ASSEMBLY_USAGE_OCCURRENCE('PRT-TQ1012-10:1','PRT-TQ1012-10:1',
'PRT-TQ1012-10:1',#33167,#33170,'PRT-TQ1012-10:1');
#147=NEXT_ASSEMBLY_USAGE_OCCURRENCE('PRT-TQ-1012-09:1',
'PRT-TQ-1012-09:1','PRT-TQ-1012-09:1',#33167,#33175,'PRT-TQ-1012-09:1');
#148=NEXT_ASSEMBLY_USAGE_OCCURRENCE('PUR-HW-4060:1','PUR-HW-4060:1',
'PUR-HW-4060:1',#33167,#33171,'PUR-HW-4060:1');
#149=NEXT_ASSEMBLY_USAGE_OCCURRENCE('PRT-TQ-1012-08:1',
'PRT-TQ-1012-08:1','PRT-TQ-1012-08:1',#33167,#33172,'PRT-TQ-1012-08:1');
#150=NEXT_ASSEMBLY_USAGE_OCCURRENCE('PRT-TQ-1012-07:1',
'PRT-TQ-1012-07:1','PRT-TQ-1012-07:1',#33167,#33173,'PRT-TQ-1012-07:1');
#151=NEXT_ASSEMBLY_USAGE_OCCURRENCE('PUR-HW-4062:1','PUR-HW-4062:1',
'PUR-HW-4062:1',#33167,#33174,'PUR-HW-4062:1');
#152=NEXT_ASSEMBLY_USAGE_OCCURRENCE('PRT-TQ-1020:1','PRT-TQ-1020:1',
'PRT-TQ-1020:1',#33167,#33176,'PRT-TQ-1020:1');
#153=NEXT_ASSEMBLY_USAGE_OCCURRENCE('PRT-TQ-1012-09:2',
'PRT-TQ-1012-09:2','PRT-TQ-1012-09:2',#33167,#33175,'PRT-TQ-1012-09:2');
#154=NEXT_ASSEMBLY_USAGE_OCCURRENCE('PRT-TQ-1012-09:3',
'PRT-TQ-1012-09:3','PRT-TQ-1012-09:3',#33167,#33175,'PRT-TQ-1012-09:3');
#155=NEXT_ASSEMBLY_USAGE_OCCURRENCE('PRT-TQ-1012-09:4',
'PRT-TQ-1012-09:4','PRT-TQ-1012-09:4',#33167,#33175,'PRT-TQ-1012-09:4');
#156=NEXT_ASSEMBLY_USAGE_OCCURRENCE('PRT-TQ-1012-09:5',
'PRT-TQ-1012-09:5','PRT-TQ-1012-09:5',#33167,#33175,'PRT-TQ-1012-09:5');
#157=NEXT_ASSEMBLY_USAGE_OCCURRENCE('PRT-TQ-1020:2','PRT-TQ-1020:2',
'PRT-TQ-1020:2',#33167,#33176,'PRT-TQ-1020:2');
#158=NEXT_ASSEMBLY_USAGE_OCCURRENCE('PRT-TQ-1012-03:1',
'PRT-TQ-1012-03:1','PRT-TQ-1012-03:1',#33178,#33179,'PRT-TQ-1012-03:1');
#159=NEXT_ASSEMBLY_USAGE_OCCURRENCE('PRT-TQ-1012-11:1',
'PRT-TQ-1012-11:1','PRT-TQ-1012-11:1',#33178,#33180,'PRT-TQ-1012-11:1');
#160=NEXT_ASSEMBLY_USAGE_OCCURRENCE('BO21-001_Ball_D3.5 Steel Ball:1',
'BO21-001_Ball_D3.5 Steel Ball:1','BO21-001_Ball_D3.5 Steel Ball:1',#33178,
#33183,'BO21-001_Ball_D3.5 Steel Ball:1');
#161=NEXT_ASSEMBLY_USAGE_OCCURRENCE('PUR-HW-4061:1','PUR-HW-4061:1',
'PUR-HW-4061:1',#33178,#33181,'PUR-HW-4061:1');
#162=NEXT_ASSEMBLY_USAGE_OCCURRENCE('PRT-TQ-1012-04:1',
'PRT-TQ-1012-04:1','PRT-TQ-1012-04:1',#33178,#33182,'PRT-TQ-1012-04:1');
#163=NEXT_ASSEMBLY_USAGE_OCCURRENCE('BO21-001_Ball_D3.5 Steel Ball:2',
'BO21-001_Ball_D3.5 Steel Ball:2','BO21-001_Ball_D3.5 Steel Ball:2',#33178,
#33183,'BO21-001_Ball_D3.5 Steel Ball:2');
#164=NEXT_ASSEMBLY_USAGE_OCCURRENCE('BO21-001_Ball_D3.5 Steel Ball:3',
'BO21-001_Ball_D3.5 Steel Ball:3','BO21-001_Ball_D3.5 Steel Ball:3',#33178,
#33183,'BO21-001_Ball_D3.5 Steel Ball:3');
#165=NEXT_ASSEMBLY_USAGE_OCCURRENCE('BO21-001_Ball_D3.5 Steel Ball:4',
'BO21-001_Ball_D3.5 Steel Ball:4','BO21-001_Ball_D3.5 Steel Ball:4',#33178,
#33183,'BO21-001_Ball_D3.5 Steel Ball:4');
#166=NEXT_ASSEMBLY_USAGE_OCCURRENCE('BO21-001_Ball_D3.5 Steel Ball:5',
'BO21-001_Ball_D3.5 Steel Ball:5','BO21-001_Ball_D3.5 Steel Ball:5',#33178,
#33183,'BO21-001_Ball_D3.5 Steel Ball:5');
#167=NEXT_ASSEMBLY_USAGE_OCCURRENCE('PRT-TQ-1012-01:1',
'PRT-TQ-1012-01:1','PRT-TQ-1012-01:1',#33156,#33157,'PRT-TQ-1012-01:1');
#168=NEXT_ASSEMBLY_USAGE_OCCURRENCE(
'S_Torque Wrench_Housing Mechanism_S_RH-1004_M_Rev01:1',
'S_Torque Wrench_Housing Mechanism_S_RH-1004_M_Rev01:1',
'S_Torque Wrench_Housing Mechanism_S_RH-1004_M_Rev01:1',#33156,#33158,
'S_Torque Wrench_Housing Mechanism_S_RH-1004_M_Rev01:1');
#169=NEXT_ASSEMBLY_USAGE_OCCURRENCE('PUR-HW-4059:1','PUR-HW-4059:1',
'PUR-HW-4059:1',#33156,#33166,'PUR-HW-4059:1');
#170=NEXT_ASSEMBLY_USAGE_OCCURRENCE(
'S_Torque Wrench_Barrel Assembly_S_Torque Wrench_Barrel Assembly_TQ-10
12_M_Rev01:1',
'S_Torque Wrench_Barrel Assembly_S_Torque Wrench_Barrel Assembly_TQ-10
12_M_Rev01:1',
'S_Torque Wrench_Barrel Assembly_S_Torque Wrench_Barrel Assembly_TQ-10
12_M_Rev01:1',#33156,#33167,
'S_Torque Wrench_Barrel Assembly_S_Torque Wrench_Barrel Assembly_TQ-10
12_M_Rev01:1');
#171=NEXT_ASSEMBLY_USAGE_OCCURRENCE('PRT-TQ-1012-14:1',
'PRT-TQ-1012-14:1','PRT-TQ-1012-14:1',#33156,#33177,'PRT-TQ-1012-14:1');
#172=NEXT_ASSEMBLY_USAGE_OCCURRENCE(
'S_Torque Wrench_Handle Grip Drive Assembly_S_Torque Wrench Handle Gri
p Drive Assembly-TQ-1012_M_Rev01:1',
'S_Torque Wrench_Handle Grip Drive Assembly_S_Torque Wrench Handle Gri
p Drive Assembly-TQ-1012_M_Rev01:1',
'S_Torque Wrench_Handle Grip Drive Assembly_S_Torque Wrench Handle Gri
p Drive Assembly-TQ-1012_M_Rev01:1',#33156,#33178,
'S_Torque Wrench_Handle Grip Drive Assembly_S_Torque Wrench Handle Gri
p Drive Assembly-TQ-1012_M_Rev01:1');
#173=NEXT_ASSEMBLY_USAGE_OCCURRENCE(
'P_Torque Wrench_Handle Grip Drive Nut_1012:1',
'P_Torque Wrench_Handle Grip Drive Nut_1012:1',
'P_Torque Wrench_Handle Grip Drive Nut_1012:1',#33156,#33186,
'P_Torque Wrench_Handle Grip Drive Nut_1012:1');
#174=NEXT_ASSEMBLY_USAGE_OCCURRENCE('PRT-TQ-1012-05:1',
'PRT-TQ-1012-05:1','PRT-TQ-1012-05:1',#33156,#33184,'PRT-TQ-1012-05:1');
#175=NEXT_ASSEMBLY_USAGE_OCCURRENCE('BO26-002_O Ring_End Cap O-ring:1',
'BO26-002_O Ring_End Cap O-ring:1','BO26-002_O Ring_End Cap O-ring:1',#33156,
#33185,'BO26-002_O Ring_End Cap O-ring:1');
#176=NEXT_ASSEMBLY_USAGE_OCCURRENCE(
'P_Torque Wrench_Handle Grip Drive Nut_1012:2',
'P_Torque Wrench_Handle Grip Drive Nut_1012:2',
'P_Torque Wrench_Handle Grip Drive Nut_1012:2',#33156,#33186,
'P_Torque Wrench_Handle Grip Drive Nut_1012:2');
#177=SPHERICAL_SURFACE('',#10689,2.75);
#178=SPHERICAL_SURFACE('',#10791,1.75);
#179=SPHERICAL_SURFACE('',#10834,5.);
#180=SPHERICAL_SURFACE('',#11148,1.75);
#181=(
BOUNDED_CURVE()
B_SPLINE_CURVE(2,(#17665,#17666,#17667),.UNSPECIFIED.,.F.,.F.)
B_SPLINE_CURVE_WITH_KNOTS((3,3),(2.46691230608693,6.35979033590771),
 .UNSPECIFIED.)
CURVE()
GEOMETRIC_REPRESENTATION_ITEM()
RATIONAL_B_SPLINE_CURVE((3.22754685436793,4.30337260646696,3.22754685436793))
REPRESENTATION_ITEM('')
);
#182=(
BOUNDED_CURVE()
B_SPLINE_CURVE(2,(#17675,#17676,#17677),.UNSPECIFIED.,.F.,.F.)
B_SPLINE_CURVE_WITH_KNOTS((3,3),(4.17496097336999,4.50967143376594),
 .UNSPECIFIED.)
CURVE()
GEOMETRIC_REPRESENTATION_ITEM()
RATIONAL_B_SPLINE_CURVE((2.9510230504805,2.95682766860845,2.9510230504805))
REPRESENTATION_ITEM('')
);
#183=(
BOUNDED_CURVE()
B_SPLINE_CURVE(2,(#17683,#17684,#17685),.UNSPECIFIED.,.F.,.F.)
B_SPLINE_CURVE_WITH_KNOTS((3,3),(2.46691230608693,6.35979033590772),
 .UNSPECIFIED.)
CURVE()
GEOMETRIC_REPRESENTATION_ITEM()
RATIONAL_B_SPLINE_CURVE((3.22754685436793,4.30337260646696,3.22754685436793))
REPRESENTATION_ITEM('')
);
#184=(
BOUNDED_CURVE()
B_SPLINE_CURVE(2,(#17691,#17692,#17693),.UNSPECIFIED.,.F.,.F.)
B_SPLINE_CURVE_WITH_KNOTS((3,3),(4.17496097336998,4.50967143376594),
 .UNSPECIFIED.)
CURVE()
GEOMETRIC_REPRESENTATION_ITEM()
RATIONAL_B_SPLINE_CURVE((2.9510230504805,2.95682766860845,2.9510230504805))
REPRESENTATION_ITEM('')
);
#185=(
BOUNDED_CURVE()
B_SPLINE_CURVE(2,(#17699,#17700,#17701),.UNSPECIFIED.,.F.,.F.)
B_SPLINE_CURVE_WITH_KNOTS((3,3),(2.46691230608693,4.41335132099732),
 .UNSPECIFIED.)
CURVE()
GEOMETRIC_REPRESENTATION_ITEM()
RATIONAL_B_SPLINE_CURVE((3.22754685436793,3.76545973041745,3.76545973041745))
REPRESENTATION_ITEM('')
);
#186=(
BOUNDED_CURVE()
B_SPLINE_CURVE(2,(#17706,#17707,#17708),.UNSPECIFIED.,.F.,.F.)
B_SPLINE_CURVE_WITH_KNOTS((3,3),(4.41335132099732,6.35979033590771),
 .UNSPECIFIED.)
CURVE()
GEOMETRIC_REPRESENTATION_ITEM()
RATIONAL_B_SPLINE_CURVE((3.76545973041745,3.76545973041745,3.22754685436793))
REPRESENTATION_ITEM('')
);
#187=(
BOUNDED_CURVE()
B_SPLINE_CURVE(2,(#17711,#17712,#17713),.UNSPECIFIED.,.F.,.F.)
B_SPLINE_CURVE_WITH_KNOTS((3,3),(4.17496097337,4.50967143376595),
 .UNSPECIFIED.)
CURVE()
GEOMETRIC_REPRESENTATION_ITEM()
RATIONAL_B_SPLINE_CURVE((2.9510230504805,2.95682766860845,2.9510230504805))
REPRESENTATION_ITEM('')
);
#188=(
BOUNDED_CURVE()
B_SPLINE_CURVE(2,(#17719,#17720,#17721),.UNSPECIFIED.,.F.,.F.)
B_SPLINE_CURVE_WITH_KNOTS((3,3),(2.46691230608693,6.35979033590771),
 .UNSPECIFIED.)
CURVE()
GEOMETRIC_REPRESENTATION_ITEM()
RATIONAL_B_SPLINE_CURVE((3.22754685436793,4.30337260646696,3.22754685436793))
REPRESENTATION_ITEM('')
);
#189=(
BOUNDED_CURVE()
B_SPLINE_CURVE(2,(#17728,#17729,#17730),.UNSPECIFIED.,.F.,.F.)
B_SPLINE_CURVE_WITH_KNOTS((3,3),(4.17496097336999,4.50967143376593),
 .UNSPECIFIED.)
CURVE()
GEOMETRIC_REPRESENTATION_ITEM()
RATIONAL_B_SPLINE_CURVE((2.9510230504805,2.95682766860845,2.9510230504805))
REPRESENTATION_ITEM('')
);
#190=(
BOUNDED_CURVE()
B_SPLINE_CURVE(2,(#18409,#18410,#18411,#18412,#18413,#18414,#18415,#18416,
#18417,#18418,#18419,#18420,#18421),.UNSPECIFIED.,.F.,.F.)
B_SPLINE_CURVE_WITH_KNOTS((3,2,2,2,2,2,3),(0.833333333333333,0.861111111111111,
0.888888888888889,0.916666666666667,0.944444444444444,0.972222222222222,
1.),.UNSPECIFIED.)
CURVE()
GEOMETRIC_REPRESENTATION_ITEM()
RATIONAL_B_SPLINE_CURVE((1.,0.866025403784439,1.,0.866025403784439,1.,0.866025403784439,
1.,0.866025403784439,1.,0.866025403784439,1.,0.866025403784439,1.))
REPRESENTATION_ITEM('')
);
#191=(
BOUNDED_CURVE()
B_SPLINE_CURVE(2,(#18423,#18424,#18425,#18426,#18427,#18428,#18429,#18430,
#18431,#18432,#18433,#18434,#18435,#18436,#18437,#18438,#18439,#18440,#18441,
#18442,#18443,#18444,#18445,#18446,#18447,#18448,#18449,#18450,#18451,#18452,
#18453,#18454,#18455,#18456,#18457,#18458,#18459,#18460,#18461,#18462,#18463,
#18464,#18465,#18466,#18467,#18468,#18469,#18470,#18471,#18472,#18473,#18474,
#18475,#18476,#18477,#18478,#18479,#18480,#18481,#18482,#18483),
 .UNSPECIFIED.,.F.,.F.)
B_SPLINE_CURVE_WITH_KNOTS((3,2,2,2,2,2,2,2,2,2,2,2,2,2,2,2,2,2,2,2,2,2,
2,2,2,2,2,2,2,2,3),(0.,0.0277777777777778,0.0555555555555556,0.0833333333333333,
0.111111111111111,0.138888888888889,0.166666666666667,0.194444444444444,
0.222222222222222,0.25,0.277777777777778,0.305555555555556,0.333333333333333,
0.361111111111111,0.388888888888889,0.416666666666667,0.444444444444444,
0.472222222222222,0.5,0.527777777777778,0.555555555555556,0.583333333333333,
0.611111111111111,0.638888888888889,0.666666666666667,0.694444444444444,
0.722222222222222,0.75,0.777777777777778,0.805555555555556,0.833333333333333),
 .UNSPECIFIED.)
CURVE()
GEOMETRIC_REPRESENTATION_ITEM()
RATIONAL_B_SPLINE_CURVE((1.,0.866025403784439,1.,0.866025403784439,1.,0.866025403784439,
1.,0.866025403784439,1.,0.866025403784439,1.,0.866025403784439,1.,0.866025403784439,
1.,0.866025403784439,1.,0.866025403784439,1.,0.866025403784439,1.,0.866025403784439,
1.,0.866025403784439,1.,0.866025403784439,1.,0.866025403784439,1.,0.866025403784439,
1.,0.866025403784439,1.,0.866025403784439,1.,0.866025403784439,1.,0.866025403784439,
1.,0.866025403784439,1.,0.866025403784439,1.,0.866025403784439,1.,0.866025403784439,
1.,0.866025403784439,1.,0.866025403784439,1.,0.866025403784439,1.,0.866025403784439,
1.,0.866025403784439,1.,0.866025403784439,1.,0.866025403784439,1.))
REPRESENTATION_ITEM('')
);
#192=(
BOUNDED_CURVE()
B_SPLINE_CURVE(2,(#18486,#18487,#18488,#18489,#18490,#18491,#18492,#18493,
#18494,#18495,#18496,#18497,#18498,#18499,#18500,#18501,#18502,#18503,#18504,
#18505,#18506,#18507,#18508,#18509,#18510,#18511,#18512,#18513,#18514,#18515,
#18516,#18517,#18518,#18519,#18520,#18521,#18522,#18523,#18524,#18525,#18526,
#18527,#18528,#18529,#18530,#18531,#18532,#18533,#18534,#18535,#18536,#18537,
#18538,#18539,#18540,#18541,#18542,#18543,#18544,#18545,#18546,#18547,#18548,
#18549,#18550,#18551,#18552,#18553,#18554,#18555,#18556,#18557,#18558),
 .UNSPECIFIED.,.F.,.F.)
B_SPLINE_CURVE_WITH_KNOTS((3,2,2,2,2,2,2,2,2,2,2,2,2,2,2,2,2,2,2,2,2,2,
2,2,2,2,2,2,2,2,2,2,2,2,2,2,3),(0.,0.0277777777777778,0.0555555555555556,
0.0833333333333333,0.111111111111111,0.138888888888889,0.166666666666667,
0.194444444444444,0.222222222222222,0.25,0.277777777777778,0.305555555555556,
0.333333333333333,0.361111111111111,0.388888888888889,0.416666666666667,
0.444444444444444,0.472222222222222,0.5,0.527777777777778,0.555555555555556,
0.583333333333333,0.611111111111111,0.638888888888889,0.666666666666667,
0.694444444444444,0.722222222222222,0.75,0.777777777777778,0.805555555555556,
0.833333333333333,0.861111111111111,0.888888888888889,0.916666666666667,
0.944444444444444,0.972222222222222,1.),.UNSPECIFIED.)
CURVE()
GEOMETRIC_REPRESENTATION_ITEM()
RATIONAL_B_SPLINE_CURVE((1.,0.866025403784439,1.,0.866025403784439,1.,0.866025403784439,
1.,0.866025403784439,1.,0.866025403784439,1.,0.866025403784439,1.,0.866025403784439,
1.,0.866025403784439,1.,0.866025403784439,1.,0.866025403784439,1.,0.866025403784439,
1.,0.866025403784439,1.,0.866025403784439,1.,0.866025403784439,1.,0.866025403784439,
1.,0.866025403784439,1.,0.866025403784439,1.,0.866025403784439,1.,0.866025403784439,
1.,0.866025403784439,1.,0.866025403784439,1.,0.866025403784439,1.,0.866025403784439,
1.,0.866025403784439,1.,0.866025403784439,1.,0.866025403784439,1.,0.866025403784439,
1.,0.866025403784439,1.,0.866025403784439,1.,0.866025403784439,1.,0.866025403784439,
1.,0.866025403784439,1.,0.866025403784439,1.,0.866025403784439,1.,0.866025403784439,
1.,0.866025403784439,1.))
REPRESENTATION_ITEM('')
);
#193=(
BOUNDED_CURVE()
B_SPLINE_CURVE(2,(#18853,#18854,#18855,#18856,#18857,#18858,#18859,#18860,
#18861,#18862,#18863,#18864,#18865),.UNSPECIFIED.,.F.,.F.)
B_SPLINE_CURVE_WITH_KNOTS((3,2,2,2,2,2,3),(0.,0.0277777777777778,0.0555555555555556,
0.0833333333333333,0.111111111111111,0.138888888888889,0.166666666666667),
 .UNSPECIFIED.)
CURVE()
GEOMETRIC_REPRESENTATION_ITEM()
RATIONAL_B_SPLINE_CURVE((1.,0.866025403784439,1.,0.866025403784439,1.,0.866025403784439,
1.,0.866025403784439,1.,0.866025403784439,1.,0.866025403784439,1.))
REPRESENTATION_ITEM('')
);
#194=(
BOUNDED_CURVE()
B_SPLINE_CURVE(2,(#18866,#18867,#18868,#18869,#18870,#18871,#18872,#18873,
#18874,#18875,#18876,#18877,#18878,#18879,#18880,#18881,#18882,#18883,#18884,
#18885,#18886,#18887,#18888,#18889,#18890,#18891,#18892,#18893,#18894,#18895,
#18896,#18897,#18898,#18899,#18900,#18901,#18902,#18903,#18904,#18905,#18906,
#18907,#18908,#18909,#18910,#18911,#18912,#18913,#18914,#18915,#18916,#18917,
#18918,#18919,#18920,#18921,#18922,#18923,#18924,#18925,#18926),
 .UNSPECIFIED.,.F.,.F.)
B_SPLINE_CURVE_WITH_KNOTS((3,2,2,2,2,2,2,2,2,2,2,2,2,2,2,2,2,2,2,2,2,2,
2,2,2,2,2,2,2,2,3),(0.,0.0277777777777778,0.0555555555555556,0.0833333333333333,
0.111111111111111,0.138888888888889,0.166666666666667,0.194444444444444,
0.222222222222222,0.25,0.277777777777778,0.305555555555556,0.333333333333333,
0.361111111111111,0.388888888888889,0.416666666666667,0.444444444444444,
0.472222222222222,0.5,0.527777777777778,0.555555555555556,0.583333333333333,
0.611111111111111,0.638888888888889,0.666666666666667,0.694444444444444,
0.722222222222222,0.75,0.777777777777778,0.805555555555556,0.833333333333333),
 .UNSPECIFIED.)
CURVE()
GEOMETRIC_REPRESENTATION_ITEM()
RATIONAL_B_SPLINE_CURVE((1.,0.866025403784439,1.,0.866025403784439,1.,0.866025403784439,
1.,0.866025403784439,1.,0.866025403784439,1.,0.866025403784439,1.,0.866025403784439,
1.,0.866025403784439,1.,0.866025403784439,1.,0.866025403784439,1.,0.866025403784439,
1.,0.866025403784439,1.,0.866025403784439,1.,0.866025403784439,1.,0.866025403784439,
1.,0.866025403784439,1.,0.866025403784439,1.,0.866025403784439,1.,0.866025403784439,
1.,0.866025403784439,1.,0.866025403784439,1.,0.866025403784439,1.,0.866025403784439,
1.,0.866025403784439,1.,0.866025403784439,1.,0.866025403784439,1.,0.866025403784439,
1.,0.866025403784439,1.,0.866025403784439,1.,0.866025403784439,1.))
REPRESENTATION_ITEM('')
);
#195=(
BOUNDED_CURVE()
B_SPLINE_CURVE(2,(#19223,#19224,#19225,#19226,#19227,#19228,#19229,#19230,
#19231,#19232,#19233,#19234,#19235,#19236,#19237,#19238,#19239,#19240,#19241,
#19242,#19243,#19244,#19245,#19246,#19247,#19248,#19249,#19250,#19251,#19252,
#19253,#19254,#19255,#19256,#19257,#19258,#19259,#19260,#19261,#19262,#19263,
#19264,#19265,#19266,#19267,#19268,#19269,#19270,#19271,#19272,#19273,#19274,
#19275,#19276,#19277,#19278,#19279,#19280,#19281,#19282,#19283,#19284,#19285,
#19286,#19287,#19288,#19289,#19290,#19291,#19292,#19293,#19294,#19295),
 .UNSPECIFIED.,.F.,.F.)
B_SPLINE_CURVE_WITH_KNOTS((3,2,2,2,2,2,2,2,2,2,2,2,2,2,2,2,2,2,2,2,2,2,
2,2,2,2,2,2,2,2,2,2,2,2,2,2,3),(0.,0.0277777777777778,0.0555555555555556,
0.0833333333333333,0.111111111111111,0.138888888888889,0.166666666666667,
0.194444444444444,0.222222222222222,0.25,0.277777777777778,0.305555555555556,
0.333333333333333,0.361111111111111,0.388888888888889,0.416666666666667,
0.444444444444444,0.472222222222222,0.5,0.527777777777778,0.555555555555556,
0.583333333333333,0.611111111111111,0.638888888888889,0.666666666666667,
0.694444444444444,0.722222222222222,0.75,0.777777777777778,0.805555555555556,
0.833333333333333,0.861111111111111,0.888888888888889,0.916666666666667,
0.944444444444444,0.972222222222222,1.),.UNSPECIFIED.)
CURVE()
GEOMETRIC_REPRESENTATION_ITEM()
RATIONAL_B_SPLINE_CURVE((1.,0.866025403784439,1.,0.866025403784439,1.,0.866025403784439,
1.,0.866025403784439,1.,0.866025403784439,1.,0.866025403784439,1.,0.866025403784439,
1.,0.866025403784439,1.,0.866025403784439,1.,0.866025403784439,1.,0.866025403784439,
1.,0.866025403784439,1.,0.866025403784439,1.,0.866025403784439,1.,0.866025403784439,
1.,0.866025403784439,1.,0.866025403784439,1.,0.866025403784439,1.,0.866025403784439,
1.,0.866025403784439,1.,0.866025403784439,1.,0.866025403784439,1.,0.866025403784439,
1.,0.866025403784439,1.,0.866025403784439,1.,0.866025403784439,1.,0.866025403784439,
1.,0.866025403784439,1.,0.866025403784439,1.,0.866025403784439,1.,0.866025403784439,
1.,0.866025403784439,1.,0.866025403784439,1.,0.866025403784439,1.,0.866025403784439,
1.,0.866025403784439,1.))
REPRESENTATION_ITEM('')
);
#196=(
BOUNDED_CURVE()
B_SPLINE_CURVE(2,(#19890,#19891,#19892,#19893,#19894,#19895,#19896,#19897,
#19898,#19899,#19900,#19901,#19902),.UNSPECIFIED.,.F.,.F.)
B_SPLINE_CURVE_WITH_KNOTS((3,2,2,2,2,2,3),(0.833333333333333,0.861111111111111,
0.888888888888889,0.916666666666667,0.944444444444444,0.972222222222222,
1.),.UNSPECIFIED.)
CURVE()
GEOMETRIC_REPRESENTATION_ITEM()
RATIONAL_B_SPLINE_CURVE((1.,0.866025403784439,1.,0.866025403784439,1.,0.866025403784439,
1.,0.866025403784439,1.,0.866025403784439,1.,0.866025403784439,1.))
REPRESENTATION_ITEM('')
);
#197=(
BOUNDED_CURVE()
B_SPLINE_CURVE(2,(#19904,#19905,#19906,#19907,#19908,#19909,#19910,#19911,
#19912,#19913,#19914,#19915,#19916,#19917,#19918,#19919,#19920,#19921,#19922,
#19923,#19924,#19925,#19926,#19927,#19928,#19929,#19930,#19931,#19932,#19933,
#19934,#19935,#19936,#19937,#19938,#19939,#19940,#19941,#19942,#19943,#19944,
#19945,#19946,#19947,#19948,#19949,#19950,#19951,#19952,#19953,#19954,#19955,
#19956,#19957,#19958,#19959,#19960,#19961,#19962,#19963,#19964),
 .UNSPECIFIED.,.F.,.F.)
B_SPLINE_CURVE_WITH_KNOTS((3,2,2,2,2,2,2,2,2,2,2,2,2,2,2,2,2,2,2,2,2,2,
2,2,2,2,2,2,2,2,3),(0.,0.0277777777777778,0.0555555555555556,0.0833333333333333,
0.111111111111111,0.138888888888889,0.166666666666667,0.194444444444444,
0.222222222222222,0.25,0.277777777777778,0.305555555555556,0.333333333333333,
0.361111111111111,0.388888888888889,0.416666666666667,0.444444444444444,
0.472222222222222,0.5,0.527777777777778,0.555555555555556,0.583333333333333,
0.611111111111111,0.638888888888889,0.666666666666667,0.694444444444444,
0.722222222222222,0.75,0.777777777777778,0.805555555555556,0.833333333333333),
 .UNSPECIFIED.)
CURVE()
GEOMETRIC_REPRESENTATION_ITEM()
RATIONAL_B_SPLINE_CURVE((1.,0.866025403784439,1.,0.866025403784439,1.,0.866025403784439,
1.,0.866025403784439,1.,0.866025403784439,1.,0.866025403784439,1.,0.866025403784439,
1.,0.866025403784439,1.,0.866025403784439,1.,0.866025403784439,1.,0.866025403784439,
1.,0.866025403784439,1.,0.866025403784439,1.,0.866025403784439,1.,0.866025403784439,
1.,0.866025403784439,1.,0.866025403784439,1.,0.866025403784439,1.,0.866025403784439,
1.,0.866025403784439,1.,0.866025403784439,1.,0.866025403784439,1.,0.866025403784439,
1.,0.866025403784439,1.,0.866025403784439,1.,0.866025403784439,1.,0.866025403784439,
1.,0.866025403784439,1.,0.866025403784439,1.,0.866025403784439,1.))
REPRESENTATION_ITEM('')
);
#198=(
BOUNDED_CURVE()
B_SPLINE_CURVE(2,(#19967,#19968,#19969,#19970,#19971,#19972,#19973,#19974,
#19975,#19976,#19977,#19978,#19979,#19980,#19981,#19982,#19983,#19984,#19985,
#19986,#19987,#19988,#19989,#19990,#19991,#19992,#19993,#19994,#19995,#19996,
#19997,#19998,#19999,#20000,#20001,#20002,#20003,#20004,#20005,#20006,#20007,
#20008,#20009,#20010,#20011,#20012,#20013,#20014,#20015,#20016,#20017,#20018,
#20019,#20020,#20021,#20022,#20023,#20024,#20025,#20026,#20027,#20028,#20029,
#20030,#20031,#20032,#20033,#20034,#20035,#20036,#20037,#20038,#20039),
 .UNSPECIFIED.,.F.,.F.)
B_SPLINE_CURVE_WITH_KNOTS((3,2,2,2,2,2,2,2,2,2,2,2,2,2,2,2,2,2,2,2,2,2,
2,2,2,2,2,2,2,2,2,2,2,2,2,2,3),(0.,0.0277777777777778,0.0555555555555556,
0.0833333333333333,0.111111111111111,0.138888888888889,0.166666666666667,
0.194444444444444,0.222222222222222,0.25,0.277777777777778,0.305555555555556,
0.333333333333333,0.361111111111111,0.388888888888889,0.416666666666667,
0.444444444444444,0.472222222222222,0.5,0.527777777777778,0.555555555555556,
0.583333333333333,0.611111111111111,0.638888888888889,0.666666666666667,
0.694444444444444,0.722222222222222,0.75,0.777777777777778,0.805555555555556,
0.833333333333333,0.861111111111111,0.888888888888889,0.916666666666667,
0.944444444444444,0.972222222222222,1.),.UNSPECIFIED.)
CURVE()
GEOMETRIC_REPRESENTATION_ITEM()
RATIONAL_B_SPLINE_CURVE((1.,0.866025403784439,1.,0.866025403784439,1.,0.866025403784439,
1.,0.866025403784439,1.,0.866025403784439,1.,0.866025403784439,1.,0.866025403784439,
1.,0.866025403784439,1.,0.866025403784439,1.,0.866025403784439,1.,0.866025403784439,
1.,0.866025403784439,1.,0.866025403784439,1.,0.866025403784439,1.,0.866025403784439,
1.,0.866025403784439,1.,0.866025403784439,1.,0.866025403784439,1.,0.866025403784439,
1.,0.866025403784439,1.,0.866025403784439,1.,0.866025403784439,1.,0.866025403784439,
1.,0.866025403784439,1.,0.866025403784439,1.,0.866025403784439,1.,0.866025403784439,
1.,0.866025403784439,1.,0.866025403784439,1.,0.866025403784439,1.,0.866025403784439,
1.,0.866025403784439,1.,0.866025403784439,1.,0.866025403784439,1.,0.866025403784439,
1.,0.866025403784439,1.))
REPRESENTATION_ITEM('')
);
#199=(
BOUNDED_CURVE()
B_SPLINE_CURVE(2,(#20334,#20335,#20336,#20337,#20338,#20339,#20340,#20341,
#20342,#20343,#20344,#20345,#20346),.UNSPECIFIED.,.F.,.F.)
B_SPLINE_CURVE_WITH_KNOTS((3,2,2,2,2,2,3),(0.,0.0277777777777778,0.0555555555555556,
0.0833333333333333,0.111111111111111,0.138888888888889,0.166666666666667),
 .UNSPECIFIED.)
CURVE()
GEOMETRIC_REPRESENTATION_ITEM()
RATIONAL_B_SPLINE_CURVE((1.,0.866025403784439,1.,0.866025403784439,1.,0.866025403784439,
1.,0.866025403784439,1.,0.866025403784439,1.,0.866025403784439,1.))
REPRESENTATION_ITEM('')
);
#200=(
BOUNDED_CURVE()
B_SPLINE_CURVE(2,(#20347,#20348,#20349,#20350,#20351,#20352,#20353,#20354,
#20355,#20356,#20357,#20358,#20359,#20360,#20361,#20362,#20363,#20364,#20365,
#20366,#20367,#20368,#20369,#20370,#20371,#20372,#20373,#20374,#20375,#20376,
#20377,#20378,#20379,#20380,#20381,#20382,#20383,#20384,#20385,#20386,#20387,
#20388,#20389,#20390,#20391,#20392,#20393,#20394,#20395,#20396,#20397,#20398,
#20399,#20400,#20401,#20402,#20403,#20404,#20405,#20406,#20407),
 .UNSPECIFIED.,.F.,.F.)
B_SPLINE_CURVE_WITH_KNOTS((3,2,2,2,2,2,2,2,2,2,2,2,2,2,2,2,2,2,2,2,2,2,
2,2,2,2,2,2,2,2,3),(0.,0.0277777777777778,0.0555555555555556,0.0833333333333333,
0.111111111111111,0.138888888888889,0.166666666666667,0.194444444444444,
0.222222222222222,0.25,0.277777777777778,0.305555555555556,0.333333333333333,
0.361111111111111,0.388888888888889,0.416666666666667,0.444444444444444,
0.472222222222222,0.5,0.527777777777778,0.555555555555556,0.583333333333333,
0.611111111111111,0.638888888888889,0.666666666666667,0.694444444444444,
0.722222222222222,0.75,0.777777777777778,0.805555555555556,0.833333333333333),
 .UNSPECIFIED.)
CURVE()
GEOMETRIC_REPRESENTATION_ITEM()
RATIONAL_B_SPLINE_CURVE((1.,0.866025403784439,1.,0.866025403784439,1.,0.866025403784439,
1.,0.866025403784439,1.,0.866025403784439,1.,0.866025403784439,1.,0.866025403784439,
1.,0.866025403784439,1.,0.866025403784439,1.,0.866025403784439,1.,0.866025403784439,
1.,0.866025403784439,1.,0.866025403784439,1.,0.866025403784439,1.,0.866025403784439,
1.,0.866025403784439,1.,0.866025403784439,1.,0.866025403784439,1.,0.866025403784439,
1.,0.866025403784439,1.,0.866025403784439,1.,0.866025403784439,1.,0.866025403784439,
1.,0.866025403784439,1.,0.866025403784439,1.,0.866025403784439,1.,0.866025403784439,
1.,0.866025403784439,1.,0.866025403784439,1.,0.866025403784439,1.))
REPRESENTATION_ITEM('')
);
#201=(
BOUNDED_CURVE()
B_SPLINE_CURVE(2,(#20704,#20705,#20706,#20707,#20708,#20709,#20710,#20711,
#20712,#20713,#20714,#20715,#20716,#20717,#20718,#20719,#20720,#20721,#20722,
#20723,#20724,#20725,#20726,#20727,#20728,#20729,#20730,#20731,#20732,#20733,
#20734,#20735,#20736,#20737,#20738,#20739,#20740,#20741,#20742,#20743,#20744,
#20745,#20746,#20747,#20748,#20749,#20750,#20751,#20752,#20753,#20754,#20755,
#20756,#20757,#20758,#20759,#20760,#20761,#20762,#20763,#20764,#20765,#20766,
#20767,#20768,#20769,#20770,#20771,#20772,#20773,#20774,#20775,#20776),
 .UNSPECIFIED.,.F.,.F.)
B_SPLINE_CURVE_WITH_KNOTS((3,2,2,2,2,2,2,2,2,2,2,2,2,2,2,2,2,2,2,2,2,2,
2,2,2,2,2,2,2,2,2,2,2,2,2,2,3),(0.,0.0277777777777778,0.0555555555555556,
0.0833333333333333,0.111111111111111,0.138888888888889,0.166666666666667,
0.194444444444444,0.222222222222222,0.25,0.277777777777778,0.305555555555556,
0.333333333333333,0.361111111111111,0.388888888888889,0.416666666666667,
0.444444444444444,0.472222222222222,0.5,0.527777777777778,0.555555555555556,
0.583333333333333,0.611111111111111,0.638888888888889,0.666666666666667,
0.694444444444444,0.722222222222222,0.75,0.777777777777778,0.805555555555556,
0.833333333333333,0.861111111111111,0.888888888888889,0.916666666666667,
0.944444444444444,0.972222222222222,1.),.UNSPECIFIED.)
CURVE()
GEOMETRIC_REPRESENTATION_ITEM()
RATIONAL_B_SPLINE_CURVE((1.,0.866025403784439,1.,0.866025403784439,1.,0.866025403784439,
1.,0.866025403784439,1.,0.866025403784439,1.,0.866025403784439,1.,0.866025403784439,
1.,0.866025403784439,1.,0.866025403784439,1.,0.866025403784439,1.,0.866025403784439,
1.,0.866025403784439,1.,0.866025403784439,1.,0.866025403784439,1.,0.866025403784439,
1.,0.866025403784439,1.,0.866025403784439,1.,0.866025403784439,1.,0.866025403784439,
1.,0.866025403784439,1.,0.866025403784439,1.,0.866025403784439,1.,0.866025403784439,
1.,0.866025403784439,1.,0.866025403784439,1.,0.866025403784439,1.,0.866025403784439,
1.,0.866025403784439,1.,0.866025403784439,1.,0.866025403784439,1.,0.866025403784439,
1.,0.866025403784439,1.,0.866025403784439,1.,0.866025403784439,1.,0.866025403784439,
1.,0.866025403784439,1.))
REPRESENTATION_ITEM('')
);
#202=(
BOUNDED_CURVE()
B_SPLINE_CURVE(2,(#27159,#27160,#27161,#27162,#27163,#27164,#27165,#27166,
#27167,#27168,#27169,#27170,#27171,#27172,#27173,#27174,#27175,#27176,#27177,
#27178,#27179,#27180,#27181,#27182,#27183,#27184,#27185,#27186,#27187,#27188,
#27189,#27190,#27191,#27192,#27193,#27194,#27195,#27196,#27197,#27198,#27199,
#27200,#27201,#27202,#27203,#27204,#27205,#27206,#27207,#27208,#27209,#27210,
#27211,#27212,#27213,#27214,#27215,#27216,#27217,#27218,#27219,#27220,#27221,
#27222,#27223,#27224,#27225,#27226,#27227,#27228,#27229,#27230,#27231,#27232,
#27233,#27234,#27235,#27236,#27237,#27238,#27239,#27240,#27241,#27242,#27243,
#27244,#27245,#27246,#27247,#27248,#27249,#27250,#27251,#27252,#27253,#27254,
#27255,#27256,#27257,#27258,#27259,#27260,#27261,#27262,#27263,#27264,#27265,
#27266,#27267,#27268,#27269,#27270,#27271,#27272,#27273,#27274,#27275,#27276,
#27277,#27278,#27279,#27280,#27281,#27282,#27283,#27284,#27285,#27286,#27287,
#27288,#27289,#27290,#27291,#27292,#27293,#27294,#27295,#27296,#27297,#27298,
#27299,#27300,#27301,#27302,#27303,#27304,#27305,#27306,#27307,#27308,#27309,
#27310,#27311,#27312,#27313,#27314,#27315,#27316,#27317,#27318,#27319,#27320,
#27321,#27322,#27323,#27324,#27325,#27326,#27327,#27328,#27329,#27330,#27331,
#27332,#27333,#27334,#27335,#27336,#27337,#27338,#27339,#27340,#27341,#27342,
#27343,#27344,#27345,#27346,#27347,#27348,#27349,#27350,#27351,#27352,#27353,
#27354,#27355,#27356,#27357,#27358,#27359,#27360,#27361,#27362,#27363,#27364,
#27365,#27366,#27367,#27368,#27369,#27370,#27371,#27372,#27373,#27374,#27375,
#27376,#27377,#27378,#27379,#27380,#27381,#27382,#27383,#27384,#27385,#27386,
#27387,#27388,#27389,#27390,#27391,#27392,#27393,#27394,#27395,#27396,#27397,
#27398,#27399,#27400,#27401,#27402,#27403,#27404,#27405,#27406,#27407,#27408,
#27409,#27410,#27411,#27412,#27413,#27414,#27415,#27416,#27417,#27418,#27419,
#27420,#27421,#27422,#27423,#27424,#27425,#27426,#27427,#27428,#27429,#27430,
#27431,#27432,#27433,#27434,#27435,#27436,#27437,#27438,#27439,#27440,#27441,
#27442,#27443,#27444,#27445,#27446,#27447,#27448,#27449,#27450,#27451,#27452,
#27453,#27454,#27455,#27456,#27457,#27458,#27459,#27460,#27461,#27462,#27463,
#27464,#27465,#27466,#27467,#27468,#27469,#27470,#27471,#27472,#27473,#27474,
#27475,#27476,#27477,#27478,#27479,#27480,#27481,#27482,#27483,#27484,#27485,
#27486,#27487,#27488,#27489,#27490,#27491,#27492,#27493,#27494,#27495,#27496,
#27497,#27498,#27499,#27500,#27501,#27502,#27503,#27504,#27505,#27506,#27507,
#27508,#27509,#27510,#27511,#27512,#27513,#27514,#27515,#27516,#27517,#27518,
#27519,#27520,#27521,#27522,#27523,#27524,#27525,#27526,#27527,#27528,#27529,
#27530,#27531,#27532,#27533,#27534,#27535,#27536,#27537,#27538,#27539,#27540,
#27541,#27542,#27543,#27544,#27545,#27546,#27547,#27548,#27549,#27550,#27551,
#27552,#27553,#27554,#27555,#27556,#27557,#27558,#27559,#27560,#27561,#27562,
#27563,#27564,#27565,#27566,#27567,#27568,#27569,#27570,#27571,#27572,#27573,
#27574,#27575,#27576,#27577,#27578,#27579,#27580,#27581,#27582,#27583,#27584,
#27585,#27586,#27587,#27588,#27589,#27590,#27591,#27592,#27593,#27594,#27595,
#27596,#27597,#27598,#27599,#27600,#27601,#27602,#27603,#27604,#27605,#27606,
#27607,#27608,#27609,#27610,#27611,#27612,#27613,#27614,#27615),
 .UNSPECIFIED.,.F.,.F.)
B_SPLINE_CURVE_WITH_KNOTS((3,2,2,2,2,2,2,2,2,2,2,2,2,2,2,2,2,2,2,2,2,2,
2,2,2,2,2,2,2,2,2,2,2,2,2,2,2,2,2,2,2,2,2,2,2,2,2,2,2,2,2,2,2,2,2,2,2,2,
2,2,2,2,2,2,2,2,2,2,2,2,2,2,2,2,2,2,2,2,2,2,2,2,2,2,2,2,2,2,2,2,2,2,2,2,
2,2,2,2,2,2,2,2,2,2,2,2,2,2,2,2,2,2,2,2,2,2,2,2,2,2,2,2,2,2,2,2,2,2,2,2,
2,2,2,2,2,2,2,2,2,2,2,2,2,2,2,2,2,2,2,2,2,2,2,2,2,2,2,2,2,2,2,2,2,2,2,2,
2,2,2,2,2,2,2,2,2,2,2,2,2,2,2,2,2,2,2,2,2,2,2,2,2,2,2,2,2,2,2,2,2,2,2,2,
2,2,2,2,2,2,2,2,2,2,2,2,2,2,2,2,2,2,2,2,2,2,2,2,2,2,3),(0.,0.0043859649122807,
0.0087719298245614,0.0131578947368421,0.0175438596491228,0.0219298245614035,
0.0263157894736842,0.0307017543859649,0.0350877192982456,0.0394736842105263,
0.043859649122807,0.0482456140350877,0.0526315789473684,0.0570175438596491,
0.0614035087719298,0.0657894736842105,0.0701754385964912,0.0745614035087719,
0.0789473684210526,0.0833333333333333,0.087719298245614,0.0921052631578947,
0.0964912280701754,0.100877192982456,0.105263157894737,0.109649122807018,
0.114035087719298,0.118421052631579,0.12280701754386,0.12719298245614,0.131578947368421,
0.135964912280702,0.140350877192982,0.144736842105263,0.149122807017544,
0.153508771929825,0.157894736842105,0.162280701754386,0.166666666666667,
0.171052631578947,0.175438596491228,0.179824561403509,0.184210526315789,
0.18859649122807,0.192982456140351,0.197368421052632,0.201754385964912,
0.206140350877193,0.210526315789474,0.214912280701754,0.219298245614035,
0.223684210526316,0.228070175438596,0.232456140350877,0.236842105263158,
0.241228070175439,0.245614035087719,0.25,0.254385964912281,0.258771929824561,
0.263157894736842,0.267543859649123,0.271929824561404,0.276315789473684,
0.280701754385965,0.285087719298246,0.289473684210526,0.293859649122807,
0.298245614035088,0.302631578947368,0.307017543859649,0.31140350877193,
0.315789473684211,0.320175438596491,0.324561403508772,0.328947368421053,
0.333333333333333,0.337719298245614,0.342105263157895,0.346491228070175,
0.350877192982456,0.355263157894737,0.359649122807018,0.364035087719298,
0.368421052631579,0.37280701754386,0.37719298245614,0.381578947368421,0.385964912280702,
0.390350877192982,0.394736842105263,0.399122807017544,0.403508771929825,
0.407894736842105,0.412280701754386,0.416666666666667,0.421052631578947,
0.425438596491228,0.429824561403509,0.434210526315789,0.43859649122807,
0.442982456140351,0.447368421052632,0.451754385964912,0.456140350877193,
0.460526315789474,0.464912280701754,0.469298245614035,0.473684210526316,
0.478070175438596,0.482456140350877,0.486842105263158,0.491228070175439,
0.495614035087719,0.5,0.504385964912281,0.508771929824561,0.513157894736842,
0.517543859649123,0.521929824561403,0.526315789473684,0.530701754385965,
0.535087719298246,0.539473684210526,0.543859649122807,0.548245614035088,
0.552631578947368,0.557017543859649,0.56140350877193,0.565789473684211,
0.570175438596491,0.574561403508772,0.578947368421053,0.583333333333333,
0.587719298245614,0.592105263157895,0.596491228070175,0.600877192982456,
0.605263157894737,0.609649122807018,0.614035087719298,0.618421052631579,
0.62280701754386,0.62719298245614,0.631578947368421,0.635964912280702,0.640350877192982,
0.644736842105263,0.649122807017544,0.653508771929825,0.657894736842105,
0.662280701754386,0.666666666666667,0.671052631578947,0.675438596491228,
0.679824561403509,0.684210526315789,0.68859649122807,0.692982456140351,
0.697368421052632,0.701754385964912,0.706140350877193,0.710526315789474,
0.714912280701754,0.719298245614035,0.723684210526316,0.728070175438597,
0.732456140350877,0.736842105263158,0.741228070175439,0.745614035087719,
0.75,0.754385964912281,0.758771929824561,0.763157894736842,0.767543859649123,
0.771929824561403,0.776315789473684,0.780701754385965,0.785087719298246,
0.789473684210526,0.793859649122807,0.798245614035088,0.802631578947368,
0.807017543859649,0.81140350877193,0.815789473684211,0.820175438596491,
0.824561403508772,0.828947368421053,0.833333333333333,0.837719298245614,
0.842105263157895,0.846491228070175,0.850877192982456,0.855263157894737,
0.859649122807018,0.864035087719298,0.868421052631579,0.87280701754386,
0.87719298245614,0.881578947368421,0.885964912280702,0.890350877192982,
0.894736842105263,0.899122807017544,0.903508771929825,0.907894736842105,
0.912280701754386,0.916666666666667,0.921052631578947,0.925438596491228,
0.929824561403509,0.934210526315789,0.93859649122807,0.942982456140351,
0.947368421052632,0.951754385964912,0.956140350877193,0.960526315789474,
0.964912280701754,0.969298245614035,0.973684210526316,0.978070175438597,
0.982456140350877,0.986842105263158,0.991228070175439,0.995614035087719,
1.),.UNSPECIFIED.)
CURVE()
GEOMETRIC_REPRESENTATION_ITEM()
RATIONAL_B_SPLINE_CURVE((1.,0.965925826289068,1.,0.965925826289068,1.,0.965925826289068,
1.,0.965925826289068,1.,0.965925826289068,1.,0.965925826289068,1.,0.965925826289068,
1.,0.965925826289068,1.,0.965925826289068,1.,0.965925826289068,1.,0.965925826289068,
1.,0.965925826289068,1.,0.965925826289068,1.,0.965925826289068,1.,0.965925826289068,
1.,0.965925826289068,1.,0.965925826289068,1.,0.965925826289068,1.,0.965925826289068,
1.,0.965925826289068,1.,0.965925826289068,1.,0.965925826289068,1.,0.965925826289068,
1.,0.965925826289068,1.,0.965925826289068,1.,0.965925826289068,1.,0.965925826289068,
1.,0.965925826289068,1.,0.965925826289068,1.,0.965925826289068,1.,0.965925826289068,
1.,0.965925826289068,1.,0.965925826289068,1.,0.965925826289068,1.,0.965925826289068,
1.,0.965925826289068,1.,0.965925826289068,1.,0.965925826289068,1.,0.965925826289068,
1.,0.965925826289068,1.,0.965925826289068,1.,0.965925826289068,1.,0.965925826289068,
1.,0.965925826289068,1.,0.965925826289068,1.,0.965925826289068,1.,0.965925826289068,
1.,0.965925826289068,1.,0.965925826289068,1.,0.965925826289068,1.,0.965925826289068,
1.,0.965925826289068,1.,0.965925826289068,1.,0.965925826289068,1.,0.965925826289068,
1.,0.965925826289068,1.,0.965925826289068,1.,0.965925826289068,1.,0.965925826289068,
1.,0.965925826289068,1.,0.965925826289068,1.,0.965925826289068,1.,0.965925826289068,
1.,0.965925826289068,1.,0.965925826289068,1.,0.965925826289068,1.,0.965925826289068,
1.,0.965925826289068,1.,0.965925826289068,1.,0.965925826289068,1.,0.965925826289068,
1.,0.965925826289068,1.,0.965925826289068,1.,0.965925826289068,1.,0.965925826289068,
1.,0.965925826289068,1.,0.965925826289068,1.,0.965925826289068,1.,0.965925826289068,
1.,0.965925826289068,1.,0.965925826289068,1.,0.965925826289068,1.,0.965925826289068,
1.,0.965925826289068,1.,0.965925826289068,1.,0.965925826289068,1.,0.965925826289068,
1.,0.965925826289068,1.,0.965925826289068,1.,0.965925826289068,1.,0.965925826289068,
1.,0.965925826289068,1.,0.965925826289068,1.,0.965925826289068,1.,0.965925826289068,
1.,0.965925826289068,1.,0.965925826289068,1.,0.965925826289068,1.,0.965925826289068,
1.,0.965925826289068,1.,0.965925826289068,1.,0.965925826289068,1.,0.965925826289068,
1.,0.965925826289068,1.,0.965925826289068,1.,0.965925826289068,1.,0.965925826289068,
1.,0.965925826289068,1.,0.965925826289068,1.,0.965925826289068,1.,0.965925826289068,
1.,0.965925826289068,1.,0.965925826289068,1.,0.965925826289068,1.,0.965925826289068,
1.,0.965925826289068,1.,0.965925826289068,1.,0.965925826289068,1.,0.965925826289068,
1.,0.965925826289068,1.,0.965925826289068,1.,0.965925826289068,1.,0.965925826289068,
1.,0.965925826289068,1.,0.965925826289068,1.,0.965925826289068,1.,0.965925826289068,
1.,0.965925826289068,1.,0.965925826289068,1.,0.965925826289068,1.,0.965925826289068,
1.,0.965925826289068,1.,0.965925826289068,1.,0.965925826289068,1.,0.965925826289068,
1.,0.965925826289068,1.,0.965925826289068,1.,0.965925826289068,1.,0.965925826289068,
1.,0.965925826289068,1.,0.965925826289068,1.,0.965925826289068,1.,0.965925826289068,
1.,0.965925826289068,1.,0.965925826289068,1.,0.965925826289068,1.,0.965925826289068,
1.,0.965925826289068,1.,0.965925826289068,1.,0.965925826289068,1.,0.965925826289068,
1.,0.965925826289068,1.,0.965925826289068,1.,0.965925826289068,1.,0.965925826289068,
1.,0.965925826289068,1.,0.965925826289068,1.,0.965925826289068,1.,0.965925826289068,
1.,0.965925826289068,1.,0.965925826289068,1.,0.965925826289068,1.,0.965925826289068,
1.,0.965925826289068,1.,0.965925826289068,1.,0.965925826289068,1.,0.965925826289068,
1.,0.965925826289068,1.,0.965925826289068,1.,0.965925826289068,1.,0.965925826289068,
1.,0.965925826289068,1.,0.965925826289068,1.,0.965925826289068,1.,0.965925826289068,
1.,0.965925826289068,1.,0.965925826289068,1.,0.965925826289068,1.,0.965925826289068,
1.,0.965925826289068,1.,0.965925826289068,1.,0.965925826289068,1.,0.965925826289068,
1.,0.965925826289068,1.,0.965925826289068,1.,0.965925826289068,1.,0.965925826289068,
1.,0.965925826289068,1.,0.965925826289068,1.,0.965925826289068,1.,0.965925826289068,
1.,0.965925826289068,1.,0.965925826289068,1.,0.965925826289068,1.,0.965925826289068,
1.,0.965925826289068,1.,0.965925826289068,1.,0.965925826289068,1.,0.965925826289068,
1.,0.965925826289068,1.,0.965925826289068,1.,0.965925826289068,1.,0.965925826289068,
1.,0.965925826289068,1.,0.965925826289068,1.,0.965925826289068,1.,0.965925826289068,
1.,0.965925826289068,1.,0.965925826289068,1.,0.965925826289068,1.,0.965925826289068,
1.,0.965925826289068,1.,0.965925826289068,1.,0.965925826289068,1.,0.965925826289068,
1.,0.965925826289068,1.,0.965925826289068,1.,0.965925826289068,1.,0.965925826289068,
1.,0.965925826289068,1.,0.965925826289068,1.,0.965925826289068,1.,0.965925826289068,
1.,0.965925826289068,1.,0.965925826289068,1.,0.965925826289068,1.,0.965925826289068,
1.,0.965925826289068,1.))
REPRESENTATION_ITEM('')
);
#203=(
BOUNDED_CURVE()
B_SPLINE_CURVE(2,(#31599,#31600,#31601,#31602,#31603,#31604,#31605,#31606,
#31607,#31608,#31609,#31610,#31611,#31612,#31613,#31614,#31615),
 .UNSPECIFIED.,.F.,.F.)
B_SPLINE_CURVE_WITH_KNOTS((3,2,2,2,2,2,2,2,3),(0.75,0.78125,0.8125,0.84375,
0.875,0.90625,0.9375,0.96875,1.),.UNSPECIFIED.)
CURVE()
GEOMETRIC_REPRESENTATION_ITEM()
RATIONAL_B_SPLINE_CURVE((1.,0.923879532511287,1.,0.923879532511287,1.,0.923879532511287,
1.,0.923879532511287,1.,0.923879532511287,1.,0.923879532511287,1.,0.923879532511287,
1.,0.923879532511287,1.))
REPRESENTATION_ITEM('')
);
#204=(
BOUNDED_CURVE()
B_SPLINE_CURVE(2,(#31617,#31618,#31619,#31620,#31621,#31622,#31623,#31624,
#31625,#31626,#31627,#31628,#31629,#31630,#31631,#31632,#31633,#31634,#31635,
#31636,#31637,#31638,#31639,#31640,#31641,#31642,#31643,#31644,#31645,#31646,
#31647,#31648,#31649,#31650,#31651,#31652,#31653,#31654,#31655,#31656,#31657,
#31658,#31659,#31660,#31661,#31662,#31663,#31664,#31665),.UNSPECIFIED.,
 .F.,.F.)
B_SPLINE_CURVE_WITH_KNOTS((3,2,2,2,2,2,2,2,2,2,2,2,2,2,2,2,2,2,2,2,2,2,
2,2,3),(0.,0.03125,0.0625,0.09375,0.125,0.15625,0.1875,0.21875,0.25,0.28125,
0.3125,0.34375,0.375,0.40625,0.4375,0.46875,0.5,0.53125,0.5625,0.59375,
0.625,0.65625,0.6875,0.71875,0.75),.UNSPECIFIED.)
CURVE()
GEOMETRIC_REPRESENTATION_ITEM()
RATIONAL_B_SPLINE_CURVE((1.,0.923879532511287,1.,0.923879532511287,1.,0.923879532511287,
1.,0.923879532511287,1.,0.923879532511287,1.,0.923879532511287,1.,0.923879532511287,
1.,0.923879532511287,1.,0.923879532511287,1.,0.923879532511287,1.,0.923879532511287,
1.,0.923879532511287,1.,0.923879532511287,1.,0.923879532511287,1.,0.923879532511287,
1.,0.923879532511287,1.,0.923879532511287,1.,0.923879532511287,1.,0.923879532511287,
1.,0.923879532511287,1.,0.923879532511287,1.,0.923879532511287,1.,0.923879532511287,
1.,0.923879532511287,1.))
REPRESENTATION_ITEM('')
);
#205=(
BOUNDED_CURVE()
B_SPLINE_CURVE(2,(#31668,#31669,#31670,#31671,#31672,#31673,#31674,#31675,
#31676,#31677,#31678,#31679,#31680,#31681,#31682,#31683,#31684,#31685,#31686,
#31687,#31688,#31689,#31690,#31691,#31692,#31693,#31694,#31695,#31696,#31697,
#31698,#31699,#31700,#31701,#31702,#31703,#31704,#31705,#31706,#31707,#31708,
#31709,#31710,#31711,#31712,#31713,#31714,#31715,#31716,#31717,#31718,#31719,
#31720,#31721,#31722,#31723,#31724,#31725,#31726,#31727,#31728,#31729,#31730,
#31731,#31732),.UNSPECIFIED.,.F.,.F.)
B_SPLINE_CURVE_WITH_KNOTS((3,2,2,2,2,2,2,2,2,2,2,2,2,2,2,2,2,2,2,2,2,2,
2,2,2,2,2,2,2,2,2,2,3),(0.,0.03125,0.0625,0.09375,0.125,0.15625,0.1875,
0.21875,0.25,0.28125,0.3125,0.34375,0.375,0.40625,0.4375,0.46875,0.5,0.53125,
0.5625,0.59375,0.625,0.65625,0.6875,0.71875,0.75,0.78125,0.8125,0.84375,
0.875,0.90625,0.9375,0.96875,1.),.UNSPECIFIED.)
CURVE()
GEOMETRIC_REPRESENTATION_ITEM()
RATIONAL_B_SPLINE_CURVE((1.,0.923879532511287,1.,0.923879532511287,1.,0.923879532511287,
1.,0.923879532511287,1.,0.923879532511287,1.,0.923879532511287,1.,0.923879532511287,
1.,0.923879532511287,1.,0.923879532511287,1.,0.923879532511287,1.,0.923879532511287,
1.,0.923879532511287,1.,0.923879532511287,1.,0.923879532511287,1.,0.923879532511287,
1.,0.923879532511287,1.,0.923879532511287,1.,0.923879532511287,1.,0.923879532511287,
1.,0.923879532511287,1.,0.923879532511287,1.,0.923879532511287,1.,0.923879532511287,
1.,0.923879532511287,1.,0.923879532511287,1.,0.923879532511287,1.,0.923879532511287,
1.,0.923879532511287,1.,0.923879532511287,1.,0.923879532511287,1.,0.923879532511287,
1.,0.923879532511287,1.))
REPRESENTATION_ITEM('')
);
#206=(
BOUNDED_CURVE()
B_SPLINE_CURVE(2,(#31995,#31996,#31997,#31998,#31999,#32000,#32001,#32002,
#32003,#32004,#32005,#32006,#32007,#32008,#32009,#32010,#32011),
 .UNSPECIFIED.,.F.,.F.)
B_SPLINE_CURVE_WITH_KNOTS((3,2,2,2,2,2,2,2,3),(0.,0.03125,0.0625,0.09375,
0.125,0.15625,0.1875,0.21875,0.25),.UNSPECIFIED.)
CURVE()
GEOMETRIC_REPRESENTATION_ITEM()
RATIONAL_B_SPLINE_CURVE((1.,0.923879532511287,1.,0.923879532511287,1.,0.923879532511287,
1.,0.923879532511287,1.,0.923879532511287,1.,0.923879532511287,1.,0.923879532511287,
1.,0.923879532511287,1.))
REPRESENTATION_ITEM('')
);
#207=(
BOUNDED_CURVE()
B_SPLINE_CURVE(2,(#32012,#32013,#32014,#32015,#32016,#32017,#32018,#32019,
#32020,#32021,#32022,#32023,#32024,#32025,#32026,#32027,#32028,#32029,#32030,
#32031,#32032,#32033,#32034,#32035,#32036,#32037,#32038,#32039,#32040,#32041,
#32042,#32043,#32044,#32045,#32046,#32047,#32048,#32049,#32050,#32051,#32052,
#32053,#32054,#32055,#32056,#32057,#32058,#32059,#32060),.UNSPECIFIED.,
 .F.,.F.)
B_SPLINE_CURVE_WITH_KNOTS((3,2,2,2,2,2,2,2,2,2,2,2,2,2,2,2,2,2,2,2,2,2,
2,2,3),(0.,0.03125,0.0625,0.09375,0.125,0.15625,0.1875,0.21875,0.25,0.28125,
0.3125,0.34375,0.375,0.40625,0.4375,0.46875,0.5,0.53125,0.5625,0.59375,
0.625,0.65625,0.6875,0.71875,0.75),.UNSPECIFIED.)
CURVE()
GEOMETRIC_REPRESENTATION_ITEM()
RATIONAL_B_SPLINE_CURVE((1.,0.923879532511287,1.,0.923879532511287,1.,0.923879532511287,
1.,0.923879532511287,1.,0.923879532511287,1.,0.923879532511287,1.,0.923879532511287,
1.,0.923879532511287,1.,0.923879532511287,1.,0.923879532511287,1.,0.923879532511287,
1.,0.923879532511287,1.,0.923879532511287,1.,0.923879532511287,1.,0.923879532511287,
1.,0.923879532511287,1.,0.923879532511287,1.,0.923879532511287,1.,0.923879532511287,
1.,0.923879532511287,1.,0.923879532511287,1.,0.923879532511287,1.,0.923879532511287,
1.,0.923879532511287,1.))
REPRESENTATION_ITEM('')
);
#208=(
BOUNDED_CURVE()
B_SPLINE_CURVE(2,(#32325,#32326,#32327,#32328,#32329,#32330,#32331,#32332,
#32333,#32334,#32335,#32336,#32337,#32338,#32339,#32340,#32341,#32342,#32343,
#32344,#32345,#32346,#32347,#32348,#32349,#32350,#32351,#32352,#32353,#32354,
#32355,#32356,#32357,#32358,#32359,#32360,#32361,#32362,#32363,#32364,#32365,
#32366,#32367,#32368,#32369,#32370,#32371,#32372,#32373,#32374,#32375,#32376,
#32377,#32378,#32379,#32380,#32381,#32382,#32383,#32384,#32385,#32386,#32387,
#32388,#32389),.UNSPECIFIED.,.F.,.F.)
B_SPLINE_CURVE_WITH_KNOTS((3,2,2,2,2,2,2,2,2,2,2,2,2,2,2,2,2,2,2,2,2,2,
2,2,2,2,2,2,2,2,2,2,3),(0.,0.03125,0.0625,0.09375,0.125,0.15625,0.1875,
0.21875,0.25,0.28125,0.3125,0.34375,0.375,0.40625,0.4375,0.46875,0.5,0.53125,
0.5625,0.59375,0.625,0.65625,0.6875,0.71875,0.75,0.78125,0.8125,0.84375,
0.875,0.90625,0.9375,0.96875,1.),.UNSPECIFIED.)
CURVE()
GEOMETRIC_REPRESENTATION_ITEM()
RATIONAL_B_SPLINE_CURVE((1.,0.923879532511287,1.,0.923879532511287,1.,0.923879532511287,
1.,0.923879532511287,1.,0.923879532511287,1.,0.923879532511287,1.,0.923879532511287,
1.,0.923879532511287,1.,0.923879532511287,1.,0.923879532511287,1.,0.923879532511287,
1.,0.923879532511287,1.,0.923879532511287,1.,0.923879532511287,1.,0.923879532511287,
1.,0.923879532511287,1.,0.923879532511287,1.,0.923879532511287,1.,0.923879532511287,
1.,0.923879532511287,1.,0.923879532511287,1.,0.923879532511287,1.,0.923879532511287,
1.,0.923879532511287,1.,0.923879532511287,1.,0.923879532511287,1.,0.923879532511287,
1.,0.923879532511287,1.,0.923879532511287,1.,0.923879532511287,1.,0.923879532511287,
1.,0.923879532511287,1.))
REPRESENTATION_ITEM('')
);
#209=(
BOUNDED_CURVE()
B_SPLINE_CURVE(2,(#32837,#32838,#32839),.UNSPECIFIED.,.F.,.F.)
B_SPLINE_CURVE_WITH_KNOTS((3,3),(-2.09220112582086,-1.49953837172718),
 .UNSPECIFIED.)
CURVE()
GEOMETRIC_REPRESENTATION_ITEM()
RATIONAL_B_SPLINE_CURVE((1.46412629524771,1.56864298547016,1.5767033028551))
REPRESENTATION_ITEM('')
);
#210=(
BOUNDED_CURVE()
B_SPLINE_CURVE(2,(#32841,#32842,#32843),.UNSPECIFIED.,.F.,.F.)
B_SPLINE_CURVE_WITH_KNOTS((3,3),(-1.40048737572359,-0.807824621629909),
 .UNSPECIFIED.)
CURVE()
GEOMETRIC_REPRESENTATION_ITEM()
RATIONAL_B_SPLINE_CURVE((1.5767033028551,1.56864298547016,1.46412629524771))
REPRESENTATION_ITEM('')
);
#211=(
BOUNDED_CURVE()
B_SPLINE_CURVE(2,(#32846,#32847,#32848),.UNSPECIFIED.,.F.,.F.)
B_SPLINE_CURVE_WITH_KNOTS((3,3),(-2.09213650825597,-1.4994860626003),
 .UNSPECIFIED.)
CURVE()
GEOMETRIC_REPRESENTATION_ITEM()
RATIONAL_B_SPLINE_CURVE((1.46410161513778,1.56861654357001,1.57667672508584))
REPRESENTATION_ITEM('')
);
#212=(
BOUNDED_CURVE()
B_SPLINE_CURVE(2,(#32849,#32850,#32851),.UNSPECIFIED.,.F.,.F.)
B_SPLINE_CURVE_WITH_KNOTS((3,3),(-1.4004371236908,-0.807786678035135),
 .UNSPECIFIED.)
CURVE()
GEOMETRIC_REPRESENTATION_ITEM()
RATIONAL_B_SPLINE_CURVE((1.57667672508584,1.56861654357001,1.46410161513778))
REPRESENTATION_ITEM('')
);
#213=(
BOUNDED_CURVE()
B_SPLINE_CURVE(2,(#32853,#32854,#32855),.UNSPECIFIED.,.F.,.F.)
B_SPLINE_CURVE_WITH_KNOTS((3,3),(-2.09220112574637,-1.49953837166687),
 .UNSPECIFIED.)
CURVE()
GEOMETRIC_REPRESENTATION_ITEM()
RATIONAL_B_SPLINE_CURVE((1.46412629521926,1.56864298543969,1.57670330282446))
REPRESENTATION_ITEM('')
);
#214=(
BOUNDED_CURVE()
B_SPLINE_CURVE(2,(#32857,#32858,#32859),.UNSPECIFIED.,.F.,.F.)
B_SPLINE_CURVE_WITH_KNOTS((3,3),(-1.40048737566568,-0.80782462158617),
 .UNSPECIFIED.)
CURVE()
GEOMETRIC_REPRESENTATION_ITEM()
RATIONAL_B_SPLINE_CURVE((1.57670330282446,1.56864298543969,1.46412629521926))
REPRESENTATION_ITEM('')
);
#215=(
BOUNDED_CURVE()
B_SPLINE_CURVE(2,(#32862,#32863,#32864),.UNSPECIFIED.,.F.,.F.)
B_SPLINE_CURVE_WITH_KNOTS((3,3),(-2.09213650825596,-1.49948606260029),
 .UNSPECIFIED.)
CURVE()
GEOMETRIC_REPRESENTATION_ITEM()
RATIONAL_B_SPLINE_CURVE((1.46410161513778,1.56861654357001,1.57667672508584))
REPRESENTATION_ITEM('')
);
#216=(
BOUNDED_CURVE()
B_SPLINE_CURVE(2,(#32865,#32866,#32867),.UNSPECIFIED.,.F.,.F.)
B_SPLINE_CURVE_WITH_KNOTS((3,3),(-1.40043712369081,-0.807786678035134),
 .UNSPECIFIED.)
CURVE()
GEOMETRIC_REPRESENTATION_ITEM()
RATIONAL_B_SPLINE_CURVE((1.57667672508584,1.56861654357001,1.46410161513778))
REPRESENTATION_ITEM('')
);
#217=(
BOUNDED_CURVE()
B_SPLINE_CURVE(2,(#32869,#32870,#32871),.UNSPECIFIED.,.F.,.F.)
B_SPLINE_CURVE_WITH_KNOTS((3,3),(-2.09220112574637,-1.49953837166686),
 .UNSPECIFIED.)
CURVE()
GEOMETRIC_REPRESENTATION_ITEM()
RATIONAL_B_SPLINE_CURVE((1.46412629521926,1.56864298543969,1.57670330282446))
REPRESENTATION_ITEM('')
);
#218=(
BOUNDED_CURVE()
B_SPLINE_CURVE(2,(#32873,#32874,#32875),.UNSPECIFIED.,.F.,.F.)
B_SPLINE_CURVE_WITH_KNOTS((3,3),(-1.40048737566568,-0.80782462158617),
 .UNSPECIFIED.)
CURVE()
GEOMETRIC_REPRESENTATION_ITEM()
RATIONAL_B_SPLINE_CURVE((1.57670330282446,1.56864298543969,1.46412629521926))
REPRESENTATION_ITEM('')
);
#219=(
BOUNDED_CURVE()
B_SPLINE_CURVE(2,(#32878,#32879,#32880),.UNSPECIFIED.,.F.,.F.)
B_SPLINE_CURVE_WITH_KNOTS((3,3),(-2.09213650825596,-1.49948606260028),
 .UNSPECIFIED.)
CURVE()
GEOMETRIC_REPRESENTATION_ITEM()
RATIONAL_B_SPLINE_CURVE((1.46410161513778,1.56861654357001,1.57667672508584))
REPRESENTATION_ITEM('')
);
#220=(
BOUNDED_CURVE()
B_SPLINE_CURVE(2,(#32881,#32882,#32883),.UNSPECIFIED.,.F.,.F.)
B_SPLINE_CURVE_WITH_KNOTS((3,3),(-1.40043712369082,-0.807786678035136),
 .UNSPECIFIED.)
CURVE()
GEOMETRIC_REPRESENTATION_ITEM()
RATIONAL_B_SPLINE_CURVE((1.57667672508584,1.56861654357001,1.46410161513778))
REPRESENTATION_ITEM('')
);
#221=(
BOUNDED_CURVE()
B_SPLINE_CURVE(2,(#32885,#32886,#32887),.UNSPECIFIED.,.F.,.F.)
B_SPLINE_CURVE_WITH_KNOTS((3,3),(-2.09220112582086,-1.49953837172717),
 .UNSPECIFIED.)
CURVE()
GEOMETRIC_REPRESENTATION_ITEM()
RATIONAL_B_SPLINE_CURVE((1.46412629524771,1.56864298547016,1.5767033028551))
REPRESENTATION_ITEM('')
);
#222=(
BOUNDED_CURVE()
B_SPLINE_CURVE(2,(#32889,#32890,#32891),.UNSPECIFIED.,.F.,.F.)
B_SPLINE_CURVE_WITH_KNOTS((3,3),(-1.4004873757236,-0.80782462162991),
 .UNSPECIFIED.)
CURVE()
GEOMETRIC_REPRESENTATION_ITEM()
RATIONAL_B_SPLINE_CURVE((1.5767033028551,1.56864298547016,1.46412629524771))
REPRESENTATION_ITEM('')
);
#223=(
BOUNDED_CURVE()
B_SPLINE_CURVE(2,(#32894,#32895,#32896),.UNSPECIFIED.,.F.,.F.)
B_SPLINE_CURVE_WITH_KNOTS((3,3),(-2.09213650825596,-1.4994860626003),
 .UNSPECIFIED.)
CURVE()
GEOMETRIC_REPRESENTATION_ITEM()
RATIONAL_B_SPLINE_CURVE((1.46410161513778,1.56861654357001,1.57667672508584))
REPRESENTATION_ITEM('')
);
#224=(
BOUNDED_CURVE()
B_SPLINE_CURVE(2,(#32897,#32898,#32899),.UNSPECIFIED.,.F.,.F.)
B_SPLINE_CURVE_WITH_KNOTS((3,3),(-1.40043712369081,-0.807786678035135),
 .UNSPECIFIED.)
CURVE()
GEOMETRIC_REPRESENTATION_ITEM()
RATIONAL_B_SPLINE_CURVE((1.57667672508584,1.56861654357001,1.46410161513778))
REPRESENTATION_ITEM('')
);
#225=(
BOUNDED_CURVE()
B_SPLINE_CURVE(2,(#32901,#32902,#32903),.UNSPECIFIED.,.F.,.F.)
B_SPLINE_CURVE_WITH_KNOTS((3,3),(-2.09220112574637,-1.49953837166688),
 .UNSPECIFIED.)
CURVE()
GEOMETRIC_REPRESENTATION_ITEM()
RATIONAL_B_SPLINE_CURVE((1.46412629521926,1.56864298543968,1.57670330282446))
REPRESENTATION_ITEM('')
);
#226=(
BOUNDED_CURVE()
B_SPLINE_CURVE(2,(#32905,#32906,#32907),.UNSPECIFIED.,.F.,.F.)
B_SPLINE_CURVE_WITH_KNOTS((3,3),(-1.40048737566567,-0.80782462158617),
 .UNSPECIFIED.)
CURVE()
GEOMETRIC_REPRESENTATION_ITEM()
RATIONAL_B_SPLINE_CURVE((1.57670330282446,1.56864298543968,1.46412629521926))
REPRESENTATION_ITEM('')
);
#227=(
BOUNDED_CURVE()
B_SPLINE_CURVE(2,(#32910,#32911,#32912),.UNSPECIFIED.,.F.,.F.)
B_SPLINE_CURVE_WITH_KNOTS((3,3),(-2.09213650825596,-1.4994860626003),
 .UNSPECIFIED.)
CURVE()
GEOMETRIC_REPRESENTATION_ITEM()
RATIONAL_B_SPLINE_CURVE((1.46410161513778,1.56861654357001,1.57667672508584))
REPRESENTATION_ITEM('')
);
#228=(
BOUNDED_CURVE()
B_SPLINE_CURVE(2,(#32913,#32914,#32915),.UNSPECIFIED.,.F.,.F.)
B_SPLINE_CURVE_WITH_KNOTS((3,3),(-1.4004371236908,-0.807786678035133),
 .UNSPECIFIED.)
CURVE()
GEOMETRIC_REPRESENTATION_ITEM()
RATIONAL_B_SPLINE_CURVE((1.57667672508584,1.56861654357001,1.46410161513778))
REPRESENTATION_ITEM('')
);
#229=(
BOUNDED_CURVE()
B_SPLINE_CURVE(2,(#32917,#32918,#32919),.UNSPECIFIED.,.F.,.F.)
B_SPLINE_CURVE_WITH_KNOTS((3,3),(-2.09220112574637,-1.49953837166687),
 .UNSPECIFIED.)
CURVE()
GEOMETRIC_REPRESENTATION_ITEM()
RATIONAL_B_SPLINE_CURVE((1.46412629521926,1.56864298543969,1.57670330282446))
REPRESENTATION_ITEM('')
);
#230=(
BOUNDED_CURVE()
B_SPLINE_CURVE(2,(#32920,#32921,#32922),.UNSPECIFIED.,.F.,.F.)
B_SPLINE_CURVE_WITH_KNOTS((3,3),(-1.40048737566567,-0.807824621586168),
 .UNSPECIFIED.)
CURVE()
GEOMETRIC_REPRESENTATION_ITEM()
RATIONAL_B_SPLINE_CURVE((1.57670330282446,1.56864298543968,1.46412629521926))
REPRESENTATION_ITEM('')
);
#231=(
BOUNDED_CURVE()
B_SPLINE_CURVE(2,(#32923,#32924,#32925),.UNSPECIFIED.,.F.,.F.)
B_SPLINE_CURVE_WITH_KNOTS((3,3),(-2.09213650825597,-1.49948606260029),
 .UNSPECIFIED.)
CURVE()
GEOMETRIC_REPRESENTATION_ITEM()
RATIONAL_B_SPLINE_CURVE((1.46410161513778,1.56861654357001,1.57667672508584))
REPRESENTATION_ITEM('')
);
#232=(
BOUNDED_CURVE()
B_SPLINE_CURVE(2,(#32926,#32927,#32928),.UNSPECIFIED.,.F.,.F.)
B_SPLINE_CURVE_WITH_KNOTS((3,3),(-1.40043712369081,-0.807786678035134),
 .UNSPECIFIED.)
CURVE()
GEOMETRIC_REPRESENTATION_ITEM()
RATIONAL_B_SPLINE_CURVE((1.57667672508584,1.56861654357001,1.46410161513778))
REPRESENTATION_ITEM('')
);
#233=SHAPE_REPRESENTATION_RELATIONSHIP('SRR','None',#33125,#260);
#234=SHAPE_REPRESENTATION_RELATIONSHIP('SRR','None',#33127,#261);
#235=SHAPE_REPRESENTATION_RELATIONSHIP('SRR','None',#33128,#262);
#236=SHAPE_REPRESENTATION_RELATIONSHIP('SRR','None',#33129,#263);
#237=SHAPE_REPRESENTATION_RELATIONSHIP('SRR','None',#33130,#264);
#238=SHAPE_REPRESENTATION_RELATIONSHIP('SRR','None',#33131,#265);
#239=SHAPE_REPRESENTATION_RELATIONSHIP('SRR','None',#33132,#266);
#240=SHAPE_REPRESENTATION_RELATIONSHIP('SRR','None',#33133,#267);
#241=SHAPE_REPRESENTATION_RELATIONSHIP('SRR','None',#33134,#268);
#242=SHAPE_REPRESENTATION_RELATIONSHIP('SRR','None',#33136,#269);
#243=SHAPE_REPRESENTATION_RELATIONSHIP('SRR','None',#33137,#270);
#244=SHAPE_REPRESENTATION_RELATIONSHIP('SRR','None',#33138,#271);
#245=SHAPE_REPRESENTATION_RELATIONSHIP('SRR','None',#33139,#272);
#246=SHAPE_REPRESENTATION_RELATIONSHIP('SRR','None',#33140,#273);
#247=SHAPE_REPRESENTATION_RELATIONSHIP('SRR','None',#33141,#274);
#248=SHAPE_REPRESENTATION_RELATIONSHIP('SRR','None',#33142,#275);
#249=SHAPE_REPRESENTATION_RELATIONSHIP('SRR','None',#33143,#276);
#250=SHAPE_REPRESENTATION_RELATIONSHIP('SRR','None',#33144,#277);
#251=SHAPE_REPRESENTATION_RELATIONSHIP('SRR','None',#33145,#278);
#252=SHAPE_REPRESENTATION_RELATIONSHIP('SRR','None',#33147,#279);
#253=SHAPE_REPRESENTATION_RELATIONSHIP('SRR','None',#33148,#280);
#254=SHAPE_REPRESENTATION_RELATIONSHIP('SRR','None',#33149,#281);
#255=SHAPE_REPRESENTATION_RELATIONSHIP('SRR','None',#33150,#282);
#256=SHAPE_REPRESENTATION_RELATIONSHIP('SRR','None',#33151,#283);
#257=SHAPE_REPRESENTATION_RELATIONSHIP('SRR','None',#33152,#284);
#258=SHAPE_REPRESENTATION_RELATIONSHIP('SRR','None',#33153,#285);
#259=SHAPE_REPRESENTATION_RELATIONSHIP('SRR','None',#33154,#286);
#260=ADVANCED_BREP_SHAPE_REPRESENTATION('',(#318),#32986);
#261=ADVANCED_BREP_SHAPE_REPRESENTATION('',(#319),#32988);
#262=ADVANCED_BREP_SHAPE_REPRESENTATION('',(#320),#32989);
#263=ADVANCED_BREP_SHAPE_REPRESENTATION('',(#321),#32990);
#264=ADVANCED_BREP_SHAPE_REPRESENTATION('',(#322),#32991);
#265=ADVANCED_BREP_SHAPE_REPRESENTATION('',(#323),#32992);
#266=ADVANCED_BREP_SHAPE_REPRESENTATION('',(#324),#32993);
#267=ADVANCED_BREP_SHAPE_REPRESENTATION('',(#325),#32994);
#268=ADVANCED_BREP_SHAPE_REPRESENTATION('',(#326),#32995);
#269=ADVANCED_BREP_SHAPE_REPRESENTATION('',(#327),#32997);
#270=ADVANCED_BREP_SHAPE_REPRESENTATION('',(#328),#32998);
#271=ADVANCED_BREP_SHAPE_REPRESENTATION('',(#329),#32999);
#272=ADVANCED_BREP_SHAPE_REPRESENTATION('',(#330),#33000);
#273=ADVANCED_BREP_SHAPE_REPRESENTATION('',(#331),#33001);
#274=ADVANCED_BREP_SHAPE_REPRESENTATION('',(#332),#33002);
#275=ADVANCED_BREP_SHAPE_REPRESENTATION('',(#333),#33003);
#276=ADVANCED_BREP_SHAPE_REPRESENTATION('',(#334),#33004);
#277=ADVANCED_BREP_SHAPE_REPRESENTATION('',(#335),#33005);
#278=ADVANCED_BREP_SHAPE_REPRESENTATION('',(#336),#33006);
#279=ADVANCED_BREP_SHAPE_REPRESENTATION('',(#337),#33008);
#280=ADVANCED_BREP_SHAPE_REPRESENTATION('',(#338),#33009);
#281=ADVANCED_BREP_SHAPE_REPRESENTATION('',(#339),#33010);
#282=ADVANCED_BREP_SHAPE_REPRESENTATION('',(#340),#33011);
#283=ADVANCED_BREP_SHAPE_REPRESENTATION('',(#341),#33012);
#284=ADVANCED_BREP_SHAPE_REPRESENTATION('',(#342),#33013);
#285=ADVANCED_BREP_SHAPE_REPRESENTATION('',(#343),#33014);
#286=ADVANCED_BREP_SHAPE_REPRESENTATION('',(#344),#33015);
#287=STYLED_ITEM('',(#33284),#318);
#288=STYLED_ITEM('',(#33284),#319);
#289=STYLED_ITEM('',(#33284),#320);
#290=STYLED_ITEM('',(#33284),#321);
#291=STYLED_ITEM('',(#33284),#322);
#292=STYLED_ITEM('',(#33285),#323);
#293=STYLED_ITEM('',(#33285),#324);
#294=STYLED_ITEM('',(#33286),#325);
#295=STYLED_ITEM('',(#33287),#326);
#296=STYLED_ITEM('',(#33284),#327);
#297=STYLED_ITEM('',(#33288),#328);
#298=STYLED_ITEM('',(#33289),#329);
#299=STYLED_ITEM('',(#33285),#330);
#300=STYLED_ITEM('',(#33289),#9712);
#301=STYLED_ITEM('',(#33289),#9713);
#302=STYLED_ITEM('',(#33289),#9714);
#303=STYLED_ITEM('',(#33289),#9722);
#304=STYLED_ITEM('',(#33288),#331);
#305=STYLED_ITEM('',(#33288),#332);
#306=STYLED_ITEM('',(#33286),#333);
#307=STYLED_ITEM('',(#33288),#334);
#308=STYLED_ITEM('',(#33288),#335);
#309=STYLED_ITEM('',(#33288),#336);
#310=STYLED_ITEM('',(#33284),#337);
#311=STYLED_ITEM('',(#33288),#338);
#312=STYLED_ITEM('',(#33285),#339);
#313=STYLED_ITEM('',(#33284),#340);
#314=STYLED_ITEM('',(#33286),#341);
#315=STYLED_ITEM('',(#33284),#342);
#316=STYLED_ITEM('',(#33287),#343);
#317=STYLED_ITEM('',(#33289),#344);
#318=MANIFOLD_SOLID_BREP('Body1',#9942);
#319=MANIFOLD_SOLID_BREP('Body1',#9943);
#320=MANIFOLD_SOLID_BREP('Body1',#9944);
#321=MANIFOLD_SOLID_BREP('Body1',#9945);
#322=MANIFOLD_SOLID_BREP('Body1',#9946);
#323=MANIFOLD_SOLID_BREP('Body1',#9947);
#324=MANIFOLD_SOLID_BREP('Body1',#9948);
#325=MANIFOLD_SOLID_BREP('Body1',#9949);
#326=MANIFOLD_SOLID_BREP('Body1',#9950);
#327=MANIFOLD_SOLID_BREP('Body1',#9951);
#328=MANIFOLD_SOLID_BREP('Body1',#9952);
#329=MANIFOLD_SOLID_BREP('Body1',#9953);
#330=MANIFOLD_SOLID_BREP('Body1',#9954);
#331=MANIFOLD_SOLID_BREP('Body1',#9955);
#332=MANIFOLD_SOLID_BREP('Body1',#9956);
#333=MANIFOLD_SOLID_BREP('Body1',#9957);
#334=MANIFOLD_SOLID_BREP('Body1',#9958);
#335=MANIFOLD_SOLID_BREP('Body1',#9959);
#336=MANIFOLD_SOLID_BREP('Body1',#9960);
#337=MANIFOLD_SOLID_BREP('Body1',#9961);
#338=MANIFOLD_SOLID_BREP('Body1',#9962);
#339=MANIFOLD_SOLID_BREP('Body1',#9963);
#340=MANIFOLD_SOLID_BREP('Body1',#9964);
#341=MANIFOLD_SOLID_BREP('Body1',#9965);
#342=MANIFOLD_SOLID_BREP('Body1',#9966);
#343=MANIFOLD_SOLID_BREP('Body1',#9967);
#344=MANIFOLD_SOLID_BREP('Body1',#9968);
#345=CONICAL_SURFACE('',#10507,8.35,0.0195779178250561);
#346=CONICAL_SURFACE('',#10575,6.08697438789325,1.13446401379632);
#347=CONICAL_SURFACE('',#10578,19.5,0.785398163397434);
#348=CONICAL_SURFACE('',#10579,5.,0.785398163397453);
#349=CONICAL_SURFACE('',#10613,3.50000000000001,0.785398163397444);
#350=CONICAL_SURFACE('',#10614,3.,0.78539816339745);
#351=CONICAL_SURFACE('',#10624,3.,0.785398163397447);
#352=CONICAL_SURFACE('',#10625,2.5,0.785398163397446);
#353=CONICAL_SURFACE('',#10660,4.50000000000001,0.785398163397445);
#354=CONICAL_SURFACE('',#10661,14.5,0.785398163397447);
#355=CONICAL_SURFACE('',#10763,9.2,0.785398163397462);
#356=CONICAL_SURFACE('',#10764,9.70000000000007,0.785398163397452);
#357=CONICAL_SURFACE('',#10765,10.6,0.785398163397424);
#358=CONICAL_SURFACE('',#10766,11.1,0.785398163397478);
#359=CONICAL_SURFACE('',#10797,2.4455,0.785398163397455);
#360=CONICAL_SURFACE('',#10976,13.,0.0282533494021236);
#361=CONICAL_SURFACE('',#10986,16.,0.785398163397441);
#362=CONICAL_SURFACE('',#10997,13.5,0.785398163397453);
#363=CONICAL_SURFACE('',#11098,6.50000000000001,1.0471975511966);
#364=CONICAL_SURFACE('',#11101,13.8985,0.785398163397456);
#365=CONICAL_SURFACE('',#11122,16.,0.244978663126864);
#366=CONICAL_SURFACE('',#11133,14.1,0.78539816339745);
#367=CONICAL_SURFACE('',#11139,13.1,0.837758040957281);
#368=CONICAL_SURFACE('',#11162,11.,1.36330010035969);
#369=CONICAL_SURFACE('',#11173,15.25,0.785398163397438);
#370=CONICAL_SURFACE('',#11174,12.3985,0.785398163397449);
#371=CONICAL_SURFACE('',#11180,9.,0.785398163397453);
#372=CONICAL_SURFACE('',#11210,6.50555349946514,0.785398163397448);
#373=CONICAL_SURFACE('',#11211,6.50555349946514,0.785398163397448);
#374=CONICAL_SURFACE('',#11212,6.50555349946514,0.785398163397448);
#375=CONICAL_SURFACE('',#11213,6.50555349946514,0.785398163397448);
#376=CONICAL_SURFACE('',#11214,6.50555349946514,0.785398163397448);
#377=CONICAL_SURFACE('',#11215,6.50555349946514,0.785398163397448);
#378=CONICAL_SURFACE('',#11216,6.50555349946514,0.785398163397448);
#379=CONICAL_SURFACE('',#11217,6.50555349946514,0.785398163397448);
#380=CONICAL_SURFACE('',#11218,6.50555349946514,0.785398163397448);
#381=CONICAL_SURFACE('',#11219,6.50555349946514,0.785398163397448);
#382=CONICAL_SURFACE('',#11220,6.50555349946514,0.785398163397448);
#383=CONICAL_SURFACE('',#11221,6.50555349946514,0.785398163397448);
#384=TOROIDAL_SURFACE('',#10492,24.,1.);
#385=TOROIDAL_SURFACE('',#10497,24.,1.);
#386=TOROIDAL_SURFACE('',#10509,10.7,2.35);
#387=TOROIDAL_SURFACE('',#10700,8.55,1.65);
#388=TOROIDAL_SURFACE('',#10729,11.375,0.8);
#389=TOROIDAL_SURFACE('',#10731,11.375,0.8);
#390=TOROIDAL_SURFACE('',#10793,4.5,0.5);
#391=TOROIDAL_SURFACE('',#10832,8.15,1.);
#392=TOROIDAL_SURFACE('',#10869,10.575,0.375000000000001);
#393=TOROIDAL_SURFACE('',#11026,4.98804347826086,0.5);
#394=TOROIDAL_SURFACE('',#11030,4.98804347826086,0.5);
#395=TOROIDAL_SURFACE('',#11033,4.98804347826086,0.5);
#396=TOROIDAL_SURFACE('',#11037,4.98804347826086,0.5);
#397=TOROIDAL_SURFACE('',#11040,4.98804347826086,0.5);
#398=TOROIDAL_SURFACE('',#11044,4.98804347826086,0.5);
#399=TOROIDAL_SURFACE('',#11048,4.98804347826086,0.5);
#400=TOROIDAL_SURFACE('',#11051,4.98804347826086,0.5);
#401=TOROIDAL_SURFACE('',#11055,4.98804347826086,0.5);
#402=TOROIDAL_SURFACE('',#11058,4.98804347826087,0.5);
#403=TOROIDAL_SURFACE('',#11099,14.5,0.5);
#404=TOROIDAL_SURFACE('',#11119,61.9943178149179,45.);
#405=TOROIDAL_SURFACE('',#11184,13.045,1.31);
#406=ELLIPSE('',#10481,60.7873002660044,48.913538415008);
#407=ELLIPSE('',#10482,61.4826185628427,49.2667804806539);
#408=ELLIPSE('',#10484,60.7873001110675,48.9135383360532);
#409=ELLIPSE('',#10485,61.4826190218256,49.2667807119994);
#410=ELLIPSE('',#11023,0.568348249767833,0.502762642635108);
#411=ELLIPSE('',#11027,0.568387932752179,0.502812488556745);
#412=ELLIPSE('',#11034,0.568387933440688,0.502812489527255);
#413=ELLIPSE('',#11041,0.568348249819522,0.502762642708099);
#414=ELLIPSE('',#11045,0.568387932758158,0.502812488561987);
#415=ELLIPSE('',#11052,0.568387932787414,0.502812488608016);
#416=(
BOUNDED_SURFACE()
B_SPLINE_SURFACE(3,2,((#16054,#16055,#16056),(#16057,#16058,#16059),(#16060,
#16061,#16062),(#16063,#16064,#16065),(#16066,#16067,#16068),(#16069,#16070,
#16071),(#16072,#16073,#16074),(#16075,#16076,#16077),(#16078,#16079,#16080),
(#16081,#16082,#16083),(#16084,#16085,#16086),(#16087,#16088,#16089),(#16090,
#16091,#16092),(#16093,#16094,#16095),(#16096,#16097,#16098),(#16099,#16100,
#16101),(#16102,#16103,#16104),(#16105,#16106,#16107),(#16108,#16109,#16110),
(#16111,#16112,#16113),(#16114,#16115,#16116),(#16117,#16118,#16119),(#16120,
#16121,#16122),(#16123,#16124,#16125),(#16126,#16127,#16128),(#16129,#16130,
#16131),(#16132,#16133,#16134),(#16135,#16136,#16137),(#16138,#16139,#16140),
(#16141,#16142,#16143),(#16144,#16145,#16146),(#16147,#16148,#16149),(#16150,
#16151,#16152),(#16153,#16154,#16155),(#16156,#16157,#16158),(#16159,#16160,
#16161)),.UNSPECIFIED.,.F.,.F.,.F.)
B_SPLINE_SURFACE_WITH_KNOTS((4,2,2,2,2,2,2,2,2,2,2,2,2,2,2,2,2,4),(3,3),
(-4.50555258903737E-5,0.00452987415304152,0.00910480383197342,0.0136797335109053,
0.0159671983503713,0.0182546631898372,0.027404522547701,0.0319794522266329,
0.0342669170660989,0.0365543819055648,0.0457042412634286,0.0502791709423605,
0.0525666357818265,0.0548541006212924,0.0640039599791562,0.0662914248186222,
0.0685788896580881,0.0731634999929292),(0.00648189094804022,1.),
 .UNSPECIFIED.)
GEOMETRIC_REPRESENTATION_ITEM()
RATIONAL_B_SPLINE_SURFACE(((1.,1.,1.),(0.999999993904585,0.999999529811955,
1.),(0.999994327863884,0.999562462855218,1.),(0.999974289583845,0.998016750330974,
1.),(0.999959924932785,0.996908690107867,1.),(0.999924657184913,0.994188207138111,
1.),(0.999903750698009,0.992575522886546,1.),(0.999868762611196,0.989876612407046,
1.),(0.999856492038748,0.988930085186398,1.),(0.999830915534174,0.986957165186696,
1.),(0.999817574138465,0.985928036818482,1.),(0.999749334292439,0.980664152670038,
1.),(0.999689814480974,0.976072914407798,1.),(0.999600229749444,0.969162528823739,
1.),(0.999570279370106,0.966852216942669,1.),(0.999525883242204,0.96342758914054,
1.),(0.999511171834468,0.962292780806495,1.),(0.999482026548572,0.960044572210512,
1.),(0.999467654311881,0.958935926847064,1.),(0.999397542938765,0.953527676872053,
1.),(0.999346550374578,0.949594213273523,1.),(0.999280801890057,0.944522507728965,
1.),(0.999260669064275,0.942969502136649,1.),(0.999233527235783,0.940875836205731,
1.),(0.999225015439781,0.940219253422205,1.),(0.999209261308267,0.939004011478145,
1.),(0.999201991019664,0.938443196072482,1.),(0.99916868183243,0.935873792521809,
1.),(0.999151750490558,0.934567742944055,1.),(0.999143044500685,0.933896180436781,
1.),(0.999141927129791,0.933809988698688,1.),(0.999140956782754,0.933735138084517,
1.),(0.999141099903996,0.933746178168636,1.),(0.999143353447026,0.933920011934732,
1.),(0.999147295336228,0.93422408132076,1.),(0.999153508906997,0.934703383643111,
1.)))
REPRESENTATION_ITEM('')
SURFACE()
);
#417=(
BOUNDED_SURFACE()
B_SPLINE_SURFACE(3,2,((#16188,#16189,#16190),(#16191,#16192,#16193),(#16194,
#16195,#16196),(#16197,#16198,#16199),(#16200,#16201,#16202),(#16203,#16204,
#16205),(#16206,#16207,#16208),(#16209,#16210,#16211),(#16212,#16213,#16214),
(#16215,#16216,#16217),(#16218,#16219,#16220),(#16221,#16222,#16223),(#16224,
#16225,#16226),(#16227,#16228,#16229)),.UNSPECIFIED.,.F.,.F.,.F.)
B_SPLINE_SURFACE_WITH_KNOTS((4,2,2,2,2,2,4),(3,3),(-3.46944695195361E-18,
0.00544424253398455,0.0108884850679691,0.0122495457014652,0.0136106063349614,
0.0163327276019537,0.0217769701359382),(0.,1.),.UNSPECIFIED.)
GEOMETRIC_REPRESENTATION_ITEM()
RATIONAL_B_SPLINE_SURFACE(((1.,0.934274323097636,1.),(1.,0.937315053619643,
1.),(1.,0.939640795315729,1.),(1.,0.942781933275843,1.),(1.,0.943598076957802,
1.),(1.,0.943602884890644,1.),(1.,0.943552641913045,1.),(1.,0.943351495816259,
1.),(1.,0.943200678675229,1.),(1.,0.942600625954464,1.),(1.,0.942003873396426,
1.),(1.,0.939645364712022,1.),(1.,0.937315936924793,1.),(1.,0.934274323097636,
1.)))
REPRESENTATION_ITEM('')
SURFACE()
);
#418=(
BOUNDED_SURFACE()
B_SPLINE_SURFACE(3,2,((#16234,#16235,#16236),(#16237,#16238,#16239),(#16240,
#16241,#16242),(#16243,#16244,#16245),(#16246,#16247,#16248),(#16249,#16250,
#16251),(#16252,#16253,#16254),(#16255,#16256,#16257),(#16258,#16259,#16260),
(#16261,#16262,#16263),(#16264,#16265,#16266),(#16267,#16268,#16269),(#16270,
#16271,#16272),(#16273,#16274,#16275),(#16276,#16277,#16278),(#16279,#16280,
#16281),(#16282,#16283,#16284),(#16285,#16286,#16287),(#16288,#16289,#16290),
(#16291,#16292,#16293),(#16294,#16295,#16296),(#16297,#16298,#16299),(#16300,
#16301,#16302),(#16303,#16304,#16305),(#16306,#16307,#16308),(#16309,#16310,
#16311),(#16312,#16313,#16314),(#16315,#16316,#16317),(#16318,#16319,#16320),
(#16321,#16322,#16323),(#16324,#16325,#16326),(#16327,#16328,#16329),(#16330,
#16331,#16332),(#16333,#16334,#16335),(#16336,#16337,#16338),(#16339,#16340,
#16341)),.UNSPECIFIED.,.F.,.F.,.F.)
B_SPLINE_SURFACE_WITH_KNOTS((4,2,2,2,2,2,2,2,2,2,2,2,2,2,2,2,2,4),(3,3),
(-4.50555258903737E-5,0.00452987415304152,0.00910480383197342,0.0136797335109053,
0.0159671983503713,0.0182546631898372,0.027404522547701,0.0319794522266329,
0.0342669170660989,0.0365543819055648,0.0457042412634286,0.0502791709423605,
0.0525666357818265,0.0548541006212924,0.0640039599791562,0.0662914248186222,
0.0685788896580881,0.0732274786700752),(0.,0.993439831725527),
 .UNSPECIFIED.)
GEOMETRIC_REPRESENTATION_ITEM()
RATIONAL_B_SPLINE_SURFACE(((1.,1.,1.),(1.,0.999999529849,0.999999993831461),
(1.,0.999562497327904,0.999994259817701),(1.,0.998016906587292,0.999973981147017),
(1.,0.996908933666058,0.999959444169404),(1.,0.994188665037773,0.999923753329497),
(1.,0.992576107846411,0.999902596036442),(1.,0.989877410008729,0.999867188212567),
(1.,0.988930957363088,0.999854770435329),(1.,0.98695819280585,0.999828887100406),
(1.,0.985929145520624,0.999815385653699),(1.,0.980665676103199,0.999746327163528),
(1.,0.976074799575539,0.99968609331843),(1.,0.969164958447091,0.999595433877325),
(1.,0.966854828590923,0.99956512419614),(1.,0.963430470608444,0.999520195466946),
(1.,0.962295751683703,0.999505307572765),(1.,0.960047720219627,0.999475812643384),
(1.,0.958939162204112,0.999461267989136),(1.,0.95353133833463,0.999390315519971),
(1.,0.949598184645746,0.999338711219874),(1.,0.944526878690836,0.999272173979003),
(1.,0.942973995456758,0.999251799628351),(1.,0.940880494481636,0.999224332190992),
(1.,0.940223963428969,0.999215718282626),(1.,0.939008817231418,0.999199775155558),
(1.,0.938448046011292,0.999192417648423),(1.,0.935878844898842,0.999158708865166),
(1.,0.934572898222151,0.999141574405253),(1.,0.933901388625957,0.999132763973354),
(1.,0.933815203678699,0.999131633197841),(1.,0.933740358961945,0.999130651209968),
(1.,0.933751398176195,0.999130796048175),(1.,0.933926836502455,0.999133097858059),
(1.,0.934237786269865,0.999137177623657),(1.,0.934728695117105,0.999143618512948)))
REPRESENTATION_ITEM('')
SURFACE()
);
#419=(
BOUNDED_SURFACE()
B_SPLINE_SURFACE(3,2,((#16362,#16363,#16364),(#16365,#16366,#16367),(#16368,
#16369,#16370),(#16371,#16372,#16373),(#16374,#16375,#16376),(#16377,#16378,
#16379),(#16380,#16381,#16382),(#16383,#16384,#16385),(#16386,#16387,#16388),
(#16389,#16390,#16391),(#16392,#16393,#16394),(#16395,#16396,#16397),(#16398,
#16399,#16400),(#16401,#16402,#16403),(#16404,#16405,#16406),(#16407,#16408,
#16409),(#16410,#16411,#16412),(#16413,#16414,#16415),(#16416,#16417,#16418),
(#16419,#16420,#16421),(#16422,#16423,#16424),(#16425,#16426,#16427),(#16428,
#16429,#16430),(#16431,#16432,#16433),(#16434,#16435,#16436),(#16437,#16438,
#16439),(#16440,#16441,#16442),(#16443,#16444,#16445),(#16446,#16447,#16448),
(#16449,#16450,#16451),(#16452,#16453,#16454),(#16455,#16456,#16457),(#16458,
#16459,#16460),(#16461,#16462,#16463),(#16464,#16465,#16466),(#16467,#16468,
#16469)),.UNSPECIFIED.,.F.,.F.,.F.)
B_SPLINE_SURFACE_WITH_KNOTS((4,2,2,2,2,2,2,2,2,2,2,2,2,2,2,2,2,4),(3,3),
(-4.50555258903755E-5,0.00452987415304115,0.00910480383197267,0.0136797335109042,
0.01596719835037,0.0182546631898357,0.0274045225476988,0.0319794522266303,
0.034266917066096,0.0365543819055618,0.0457042412634248,0.0502791709423564,
0.0525666357818221,0.0548541006212879,0.0640039599791509,0.0662914248186167,
0.0685788896580825,0.0732274786569346),(0.,0.993439832057625),
 .UNSPECIFIED.)
GEOMETRIC_REPRESENTATION_ITEM()
RATIONAL_B_SPLINE_SURFACE(((1.,1.,1.),(1.,0.999999529849,0.999999993831461),
(1.,0.999562497327757,0.99999425981799),(1.,0.998016906586629,0.999973981148326),
(1.,0.996908933665109,0.999959444171444),(1.,0.994188665035747,0.99992375333333),
(1.,0.992576107844015,0.999902596041341),(1.,0.989877410005303,0.999867188219246),
(1.,0.988930957359389,0.999854770442633),(1.,0.986958192801492,0.999828887109012),
(1.,0.985929145515922,0.999815385662983),(1.,0.980665676096738,0.999746327176285),
(1.,0.976074799567374,0.999686093334214),(1.,0.969164958436868,0.999595433897671),
(1.,0.96685482857993,0.999565124218011),(1.,0.963430470596179,0.999520195491075),
(1.,0.962295751671145,0.999505307597643),(1.,0.960047720206233,0.999475812669744),
(1.,0.958939162190388,0.999461268016229),(1.,0.953531338319099,0.999390315550632),
(1.,0.949598184628729,0.999338711253128),(1.,0.944526878672376,0.999272174015606),
(1.,0.942973995437611,0.999251799665976),(1.,0.940880494461918,0.99922433223),
(1.,0.940223963408945,0.999215718322066),(1.,0.939008817211073,0.999199775195801),
(1.,0.938448045990673,0.999192417689035),(1.,0.935878844877576,0.999158708907476),
(1.,0.934572898200279,0.999141574448422),(1.,0.933901388603861,0.999132764016967),
(1.,0.933815203656616,0.999131633241511),(1.,0.933740358939752,0.999130651253686),
(1.,0.933751398154091,0.999130796091887),(1.,0.933926836479949,0.999133097901649),
(1.,0.934237786246193,0.999137177667025),(1.,0.934728695091121,0.999143618555959)))
REPRESENTATION_ITEM('')
SURFACE()
);
#420=(
BOUNDED_SURFACE()
B_SPLINE_SURFACE(3,2,((#16492,#16493,#16494),(#16495,#16496,#16497),(#16498,
#16499,#16500),(#16501,#16502,#16503),(#16504,#16505,#16506),(#16507,#16508,
#16509),(#16510,#16511,#16512),(#16513,#16514,#16515),(#16516,#16517,#16518),
(#16519,#16520,#16521),(#16522,#16523,#16524),(#16525,#16526,#16527),(#16528,
#16529,#16530),(#16531,#16532,#16533)),.UNSPECIFIED.,.F.,.F.,.F.)
B_SPLINE_SURFACE_WITH_KNOTS((4,2,2,2,2,2,4),(3,3),(-1.38777878078145E-17,
0.00544424253398438,0.0108884850679688,0.0122495457014649,0.013610606334961,
0.0163327276019532,0.0217769701359376),(0.,1.),.UNSPECIFIED.)
GEOMETRIC_REPRESENTATION_ITEM()
RATIONAL_B_SPLINE_SURFACE(((1.,0.934274323097636,1.),(1.,0.937315053619719,
1.),(1.,0.939640795315628,1.),(1.,0.942781933275944,1.),(1.,0.943598076957802,
1.),(1.,0.943602884890644,1.),(1.,0.943552641913071,1.),(1.,0.943351495816233,
1.),(1.,0.943200678675229,1.),(1.,0.942600625954464,1.),(1.,0.942003873396376,
1.),(1.,0.939645364712124,1.),(1.,0.937315936924713,1.),(1.,0.934274323097642,
1.)))
REPRESENTATION_ITEM('')
SURFACE()
);
#421=(
BOUNDED_SURFACE()
B_SPLINE_SURFACE(3,2,((#16538,#16539,#16540),(#16541,#16542,#16543),(#16544,
#16545,#16546),(#16547,#16548,#16549),(#16550,#16551,#16552),(#16553,#16554,
#16555),(#16556,#16557,#16558),(#16559,#16560,#16561),(#16562,#16563,#16564),
(#16565,#16566,#16567),(#16568,#16569,#16570),(#16571,#16572,#16573),(#16574,
#16575,#16576),(#16577,#16578,#16579),(#16580,#16581,#16582),(#16583,#16584,
#16585),(#16586,#16587,#16588),(#16589,#16590,#16591),(#16592,#16593,#16594),
(#16595,#16596,#16597),(#16598,#16599,#16600),(#16601,#16602,#16603),(#16604,
#16605,#16606),(#16607,#16608,#16609),(#16610,#16611,#16612),(#16613,#16614,
#16615),(#16616,#16617,#16618),(#16619,#16620,#16621),(#16622,#16623,#16624),
(#16625,#16626,#16627),(#16628,#16629,#16630),(#16631,#16632,#16633),(#16634,
#16635,#16636),(#16637,#16638,#16639),(#16640,#16641,#16642),(#16643,#16644,
#16645)),.UNSPECIFIED.,.F.,.F.,.F.)
B_SPLINE_SURFACE_WITH_KNOTS((4,2,2,2,2,2,2,2,2,2,2,2,2,2,2,2,2,4),(3,3),
(-4.50555258903699E-5,0.00452987415304452,0.00910480383197942,0.0136797335109143,
0.0159671983503818,0.0182546631898492,0.027404522547719,0.0319794522266539,
0.0342669170661213,0.0365543819055888,0.0457042412634586,0.0502791709423935,
0.0525666357818609,0.0548541006213284,0.0640039599791982,0.0662914248186656,
0.0685788896581331,0.0731634999929532),(0.00648190587163059,1.),
 .UNSPECIFIED.)
GEOMETRIC_REPRESENTATION_ITEM()
RATIONAL_B_SPLINE_SURFACE(((1.,1.,1.),(0.999999993904571,0.999999529811961,
1.),(0.99999432785091,0.99956246286179,1.),(0.999974289525037,0.998016750360764,
1.),(0.99995992484112,0.996908690154303,1.),(0.999924657012579,0.994188207225404,
1.),(0.999903750477856,0.992575522998147,1.),(0.999868762311012,0.989876612559059,
1.),(0.999856491710498,0.98893008535267,1.),(0.999830915147422,0.986957165382596,
1.),(0.999817573721197,0.985928037029841,1.),(0.999749333719083,0.98066415296048,
1.),(0.999689813771477,0.976072914767201,1.),(0.999600228835038,0.969162529286938,
1.),(0.999570278387192,0.966852217440492,1.),(0.999525882157743,0.963427589689905,
1.),(0.999511170716356,0.962292781372864,1.),(0.999482025363796,0.960044572810649,
1.),(0.99946765309423,0.958935927463858,1.),(0.999397541560747,0.953527677570119,
1.),(0.999346548879922,0.949594214030664,1.),(0.999280800245013,0.944522508562285,
1.),(0.999260667373182,0.942969502993375,1.),(0.999233525482606,0.940875837093776,
1.),(0.999225013667134,0.940219254320119,1.),(0.999209259499587,0.939004012394397,
1.),(0.999201989194353,0.938443196997076,1.),(0.999168679930933,0.935873793485225,
1.),(0.999151748550332,0.93456774392691,1.),(0.999143042540544,0.933896181429722,
1.),(0.999141925167095,0.933809989692925,1.),(0.999140954817838,0.933735139079878,
1.),(0.999141097939409,0.933746179163875,1.),(0.999143351487591,0.933920012927231,
1.),(0.999147293385812,0.934224082308839,1.),(0.999153506970792,0.93470338462392,
1.)))
REPRESENTATION_ITEM('')
SURFACE()
);
#422=(
BOUNDED_SURFACE()
B_SPLINE_SURFACE(3,2,((#16675,#16676,#16677),(#16678,#16679,#16680),(#16681,
#16682,#16683),(#16684,#16685,#16686),(#16687,#16688,#16689),(#16690,#16691,
#16692),(#16693,#16694,#16695),(#16696,#16697,#16698),(#16699,#16700,#16701),
(#16702,#16703,#16704),(#16705,#16706,#16707),(#16708,#16709,#16710),(#16711,
#16712,#16713),(#16714,#16715,#16716),(#16717,#16718,#16719),(#16720,#16721,
#16722),(#16723,#16724,#16725),(#16726,#16727,#16728),(#16729,#16730,#16731),
(#16732,#16733,#16734)),.UNSPECIFIED.,.F.,.F.,.F.)
B_SPLINE_SURFACE_WITH_KNOTS((4,2,2,2,2,2,2,2,2,4),(3,3),(-1.21430643318376E-17,
0.000286716408612401,0.000573432817224815,0.00114686563444964,0.00229373126889929,
0.0045874625377986,0.00688119380669791,0.00917492507559722,0.0137623876133958,
0.0183498501511944),(0.,1.),.UNSPECIFIED.)
GEOMETRIC_REPRESENTATION_ITEM()
RATIONAL_B_SPLINE_SURFACE(((1.,0.715678085420542,1.),(1.,0.732713574734388,
1.),(1.,0.751287941176003,1.),(1.,0.783048929818799,1.),(1.,0.796213241095476,
1.),(1.,0.829148860260418,1.),(1.,0.843569652884034,1.),(1.,0.879829452120598,
1.),(1.,0.894194157570232,1.),(1.,0.930380052244755,1.),(1.,0.943334851348775,
1.),(1.,0.964070509897579,1.),(1.,0.97097877739709,1.),(1.,0.98166631964498,
1.),(1.,0.985389932826228,1.),(1.,0.994077955423915,1.),(1.,0.996586035113217,
1.),(1.,0.999617313053908,1.),(1.,0.999976096727813,1.),(1.,1.,1.)))
REPRESENTATION_ITEM('')
SURFACE()
);
#423=(
BOUNDED_SURFACE()
B_SPLINE_SURFACE(3,2,((#16736,#16737,#16738),(#16739,#16740,#16741),(#16742,
#16743,#16744),(#16745,#16746,#16747)),.UNSPECIFIED.,.F.,.F.,.F.)
B_SPLINE_SURFACE_WITH_KNOTS((4,4),(3,3),(0.,0.00310259288126481),(0.,1.),
 .UNSPECIFIED.)
GEOMETRIC_REPRESENTATION_ITEM()
RATIONAL_B_SPLINE_SURFACE(((1.,0.707106781186544,1.),(1.,0.709735448065174,
1.),(1.,0.712575844075049,1.),(1.,0.715678085420518,1.)))
REPRESENTATION_ITEM('')
SURFACE()
);
#424=(
BOUNDED_SURFACE()
B_SPLINE_SURFACE(3,2,((#16751,#16752,#16753),(#16754,#16755,#16756),(#16757,
#16758,#16759),(#16760,#16761,#16762)),.UNSPECIFIED.,.F.,.F.,.F.)
B_SPLINE_SURFACE_WITH_KNOTS((4,4),(3,3),(-1.73472347597681E-18,0.00310259288126371),
(0.,1.),.UNSPECIFIED.)
GEOMETRIC_REPRESENTATION_ITEM()
RATIONAL_B_SPLINE_SURFACE(((1.,0.715678085420547,1.),(1.,0.712575844075018,
1.),(1.,0.709735448065194,1.),(1.,0.707106781186547,1.)))
REPRESENTATION_ITEM('')
SURFACE()
);
#425=(
BOUNDED_SURFACE()
B_SPLINE_SURFACE(3,2,((#16764,#16765,#16766),(#16767,#16768,#16769),(#16770,
#16771,#16772),(#16773,#16774,#16775),(#16776,#16777,#16778),(#16779,#16780,
#16781),(#16782,#16783,#16784),(#16785,#16786,#16787),(#16788,#16789,#16790),
(#16791,#16792,#16793),(#16794,#16795,#16796),(#16797,#16798,#16799),(#16800,
#16801,#16802),(#16803,#16804,#16805),(#16806,#16807,#16808),(#16809,#16810,
#16811),(#16812,#16813,#16814),(#16815,#16816,#16817),(#16818,#16819,#16820),
(#16821,#16822,#16823),(#16824,#16825,#16826),(#16827,#16828,#16829)),
 .UNSPECIFIED.,.F.,.F.,.F.)
B_SPLINE_SURFACE_WITH_KNOTS((4,2,2,2,2,2,2,2,2,2,4),(3,3),(-4.45822180120765E-5,
0.00456146106532619,0.00686448270699533,0.00916750434866446,0.0114705259903336,
0.0137735476320027,0.0160765692736719,0.0172280800945064,0.0178038355049237,
0.0180917132101324,0.018655949664608),(0.,1.00027635874927),
 .UNSPECIFIED.)
GEOMETRIC_REPRESENTATION_ITEM()
RATIONAL_B_SPLINE_SURFACE(((1.,1.,1.),(1.,0.999975269355394,1.00000001366906),
(1.,0.999616856262281,1.00000021177025),(1.,0.997367139234066,1.00000145522822),
(1.,0.996329945283138,1.00000202850346),(1.,0.993242400650488,1.00000373504341),
(1.,0.991218555061358,1.00000485365828),(1.,0.985482929988757,1.00000802383862),
(1.,0.981797060269541,1.00001006108331),(1.,0.971222431433512,1.00001590586571),
(1.,0.964447640919971,1.00001965041098),(1.,0.943699466562788,1.00003111829001),
(1.,0.930712139865289,1.00003829661273),(1.,0.89444331730149,1.00005834302561),
(1.,0.880044194752108,1.00006630167261),(1.,0.843708864884983,1.00008638484524),
(1.,0.82925954511809,1.00009437123712),(1.,0.796263056814172,1.0001126089736),
(1.,0.783074395977812,1.00011989857722),(1.,0.735984363806146,1.00014592606201),
(1.,0.694442358121852,1.00016888705548),(1.,0.674552380648109,1.00017988059407)))
REPRESENTATION_ITEM('')
SURFACE()
);
#426=(
BOUNDED_SURFACE()
B_SPLINE_SURFACE(3,2,((#16830,#16831,#16832),(#16833,#16834,#16835),(#16836,
#16837,#16838),(#16839,#16840,#16841),(#16842,#16843,#16844),(#16845,#16846,
#16847),(#16848,#16849,#16850),(#16851,#16852,#16853),(#16854,#16855,#16856),
(#16857,#16858,#16859),(#16860,#16861,#16862),(#16863,#16864,#16865),(#16866,
#16867,#16868),(#16869,#16870,#16871),(#16872,#16873,#16874),(#16875,#16876,
#16877),(#16878,#16879,#16880),(#16881,#16882,#16883),(#16884,#16885,#16886),
(#16887,#16888,#16889),(#16890,#16891,#16892),(#16893,#16894,#16895)),
 .UNSPECIFIED.,.F.,.F.,.F.)
B_SPLINE_SURFACE_WITH_KNOTS((4,2,2,2,2,2,2,2,2,2,4),(3,3),(-4.45822180121706E-5,
0.00228108920328879,0.00460676062458975,0.00925810346719167,0.0115837748884926,
0.0139094463097936,0.0162351177310945,0.017397953441745,0.0179793712970703,
0.0182700802247329,0.0185607891523955),(0.,1.),.UNSPECIFIED.)
GEOMETRIC_REPRESENTATION_ITEM()
RATIONAL_B_SPLINE_SURFACE(((1.,1.,1.),(1.,0.999998791721631,1.),(1.,0.999892445298426,
1.),(1.,0.999316761910651,1.),(1.,0.998852418425575,1.),(1.,0.996589788033769,
1.),(1.,0.994126671587873,1.),(1.,0.985446396309632,1.),(1.,0.981713646123456,
1.),(1.,0.971107052837317,1.),(1.,0.96432827074271,1.),(1.,0.943870035476799,
1.),(1.,0.931100277618097,1.),(1.,0.894796160803365,1.),(1.,0.88026171681454,
1.),(1.,0.843728071613052,1.),(1.,0.829200458708476,1.),(1.,0.796111926064673,
1.),(1.,0.782895634776705,1.),(1.,0.751122556026189,1.),(1.,0.732604759639831,
1.),(1.,0.715678085420547,1.)))
REPRESENTATION_ITEM('')
SURFACE()
);
#427=(
BOUNDED_SURFACE()
B_SPLINE_SURFACE(3,2,((#16897,#16898,#16899),(#16900,#16901,#16902),(#16903,
#16904,#16905),(#16906,#16907,#16908)),.UNSPECIFIED.,.F.,.F.,.F.)
B_SPLINE_SURFACE_WITH_KNOTS((4,4),(3,3),(0.,0.00310259288127954),(0.,1.),
 .UNSPECIFIED.)
GEOMETRIC_REPRESENTATION_ITEM()
RATIONAL_B_SPLINE_SURFACE(((1.,0.715678085420547,1.),(1.,0.712575844075105,
1.),(1.,0.709735448065179,1.),(1.,0.707106781186548,1.)))
REPRESENTATION_ITEM('')
SURFACE()
);
#428=(
BOUNDED_SURFACE()
B_SPLINE_SURFACE(3,2,((#16912,#16913,#16914),(#16915,#16916,#16917),(#16918,
#16919,#16920),(#16921,#16922,#16923)),.UNSPECIFIED.,.F.,.F.,.F.)
B_SPLINE_SURFACE_WITH_KNOTS((4,4),(3,3),(0.,0.00310259288126651),(0.,1.),
 .UNSPECIFIED.)
GEOMETRIC_REPRESENTATION_ITEM()
RATIONAL_B_SPLINE_SURFACE(((1.,0.70710678118654,1.),(1.,0.709735448065188,
1.),(1.,0.712575844075016,1.),(1.,0.715678085420547,1.)))
REPRESENTATION_ITEM('')
SURFACE()
);
#429=(
BOUNDED_SURFACE()
B_SPLINE_SURFACE(3,2,((#16925,#16926,#16927),(#16928,#16929,#16930),(#16931,
#16932,#16933),(#16934,#16935,#16936),(#16937,#16938,#16939),(#16940,#16941,
#16942),(#16943,#16944,#16945),(#16946,#16947,#16948),(#16949,#16950,#16951),
(#16952,#16953,#16954),(#16955,#16956,#16957),(#16958,#16959,#16960),(#16961,
#16962,#16963),(#16964,#16965,#16966),(#16967,#16968,#16969),(#16970,#16971,
#16972),(#16973,#16974,#16975),(#16976,#16977,#16978),(#16979,#16980,#16981),
(#16982,#16983,#16984)),.UNSPECIFIED.,.F.,.F.,.F.)
B_SPLINE_SURFACE_WITH_KNOTS((4,2,2,2,2,2,2,2,2,4),(3,3),(0.,0.000286716408612405,
0.00057343281722481,0.00114686563444962,0.00229373126889924,0.00458746253779848,
0.00688119380669772,0.00917492507559696,0.0137623876133954,0.0183498501511939),
(0.,1.),.UNSPECIFIED.)
GEOMETRIC_REPRESENTATION_ITEM()
RATIONAL_B_SPLINE_SURFACE(((1.,0.715678085420547,1.),(1.,0.732713574734547,
1.),(1.,0.751287941176143,1.),(1.,0.783048929818852,1.),(1.,0.796213241095647,
1.),(1.,0.829148860260267,1.),(1.,0.843569652884057,1.),(1.,0.879829452120653,
1.),(1.,0.894194157570376,1.),(1.,0.930380052244515,1.),(1.,0.943334851348824,
1.),(1.,0.964070509897542,1.),(1.,0.970978777396964,1.),(1.,0.981666319645111,
1.),(1.,0.985389932826229,1.),(1.,0.994077955423916,1.),(1.,0.996586035113046,
1.),(1.,0.99961731305408,1.),(1.,0.999976096727683,1.),(1.,1.,1.)))
REPRESENTATION_ITEM('')
SURFACE()
);
#430=(
BOUNDED_SURFACE()
B_SPLINE_SURFACE(2,2,((#16994,#16995,#16996,#16997,#16998,#16999,#17000,
#17001,#17002),(#17003,#17004,#17005,#17006,#17007,#17008,#17009,#17010,
#17011),(#17012,#17013,#17014,#17015,#17016,#17017,#17018,#17019,#17020)),
 .UNSPECIFIED.,.F.,.T.,.F.)
B_SPLINE_SURFACE_WITH_KNOTS((3,3),(3,2,2,2,3),(-0.442628884695582,0.442628884695581),
(-3.14159265358979,-1.5707963267949,0.,1.5707963267949,3.14159265358979),
 .UNSPECIFIED.)
GEOMETRIC_REPRESENTATION_ITEM()
RATIONAL_B_SPLINE_SURFACE(((1.,0.707106781186548,1.,0.707106781186548,1.,
0.707106781186548,1.,0.707106781186548,1.),(0.903628792385486,0.638962046771188,
0.903628792385486,0.638962046771188,0.903628792385486,0.638962046771188,
0.903628792385486,0.638962046771188,0.903628792385486),(1.,0.707106781186548,
1.,0.707106781186548,1.,0.707106781186548,1.,0.707106781186548,1.)))
REPRESENTATION_ITEM('')
SURFACE()
);
#431=(
BOUNDED_SURFACE()
B_SPLINE_SURFACE(3,2,((#18113,#18114,#18115,#18116,#18117,#18118,#18119,
#18120,#18121,#18122,#18123,#18124,#18125,#18126,#18127,#18128,#18129,#18130,
#18131,#18132,#18133,#18134,#18135,#18136,#18137,#18138,#18139,#18140,#18141,
#18142,#18143,#18144,#18145,#18146,#18147,#18148,#18149,#18150,#18151,#18152,
#18153,#18154,#18155,#18156,#18157,#18158,#18159,#18160,#18161,#18162,#18163,
#18164,#18165,#18166,#18167,#18168,#18169,#18170,#18171,#18172,#18173,#18174,
#18175,#18176,#18177,#18178,#18179,#18180,#18181,#18182,#18183,#18184,#18185),
(#18186,#18187,#18188,#18189,#18190,#18191,#18192,#18193,#18194,#18195,
#18196,#18197,#18198,#18199,#18200,#18201,#18202,#18203,#18204,#18205,#18206,
#18207,#18208,#18209,#18210,#18211,#18212,#18213,#18214,#18215,#18216,#18217,
#18218,#18219,#18220,#18221,#18222,#18223,#18224,#18225,#18226,#18227,#18228,
#18229,#18230,#18231,#18232,#18233,#18234,#18235,#18236,#18237,#18238,#18239,
#18240,#18241,#18242,#18243,#18244,#18245,#18246,#18247,#18248,#18249,#18250,
#18251,#18252,#18253,#18254,#18255,#18256,#18257,#18258),(#18259,#18260,
#18261,#18262,#18263,#18264,#18265,#18266,#18267,#18268,#18269,#18270,#18271,
#18272,#18273,#18274,#18275,#18276,#18277,#18278,#18279,#18280,#18281,#18282,
#18283,#18284,#18285,#18286,#18287,#18288,#18289,#18290,#18291,#18292,#18293,
#18294,#18295,#18296,#18297,#18298,#18299,#18300,#18301,#18302,#18303,#18304,
#18305,#18306,#18307,#18308,#18309,#18310,#18311,#18312,#18313,#18314,#18315,
#18316,#18317,#18318,#18319,#18320,#18321,#18322,#18323,#18324,#18325,#18326,
#18327,#18328,#18329,#18330,#18331),(#18332,#18333,#18334,#18335,#18336,
#18337,#18338,#18339,#18340,#18341,#18342,#18343,#18344,#18345,#18346,#18347,
#18348,#18349,#18350,#18351,#18352,#18353,#18354,#18355,#18356,#18357,#18358,
#18359,#18360,#18361,#18362,#18363,#18364,#18365,#18366,#18367,#18368,#18369,
#18370,#18371,#18372,#18373,#18374,#18375,#18376,#18377,#18378,#18379,#18380,
#18381,#18382,#18383,#18384,#18385,#18386,#18387,#18388,#18389,#18390,#18391,
#18392,#18393,#18394,#18395,#18396,#18397,#18398,#18399,#18400,#18401,#18402,
#18403,#18404)),.UNSPECIFIED.,.F.,.F.,.F.)
B_SPLINE_SURFACE_WITH_KNOTS((4,4),(3,2,2,2,2,2,2,2,2,2,2,2,2,2,2,2,2,2,
2,2,2,2,2,2,2,2,2,2,2,2,2,2,2,2,2,2,3),(0.,1.),(0.,0.0277777777777778,0.0555555555555556,
0.0833333333333333,0.111111111111111,0.138888888888889,0.166666666666667,
0.194444444444444,0.222222222222222,0.25,0.277777777777778,0.305555555555556,
0.333333333333333,0.361111111111111,0.388888888888889,0.416666666666667,
0.444444444444444,0.472222222222222,0.5,0.527777777777778,0.555555555555556,
0.583333333333333,0.611111111111111,0.638888888888889,0.666666666666667,
0.694444444444444,0.722222222222222,0.75,0.777777777777778,0.805555555555556,
0.833333333333333,0.861111111111111,0.888888888888889,0.916666666666667,
0.944444444444444,0.972222222222222,1.),.UNSPECIFIED.)
GEOMETRIC_REPRESENTATION_ITEM()
RATIONAL_B_SPLINE_SURFACE(((1.,0.866025403784439,1.,0.866025403784439,1.,
0.866025403784439,1.,0.866025403784439,1.,0.866025403784439,1.,0.866025403784439,
1.,0.866025403784439,1.,0.866025403784439,1.,0.866025403784439,1.,0.866025403784439,
1.,0.866025403784439,1.,0.866025403784439,1.,0.866025403784439,1.,0.866025403784439,
1.,0.866025403784439,1.,0.866025403784439,1.,0.866025403784439,1.,0.866025403784439,
1.,0.866025403784439,1.,0.866025403784439,1.,0.866025403784439,1.,0.866025403784439,
1.,0.866025403784439,1.,0.866025403784439,1.,0.866025403784439,1.,0.866025403784439,
1.,0.866025403784439,1.,0.866025403784439,1.,0.866025403784439,1.,0.866025403784439,
1.,0.866025403784439,1.,0.866025403784439,1.,0.866025403784439,1.,0.866025403784439,
1.,0.866025403784439,1.,0.866025403784439,1.),(0.804737854124365,0.696923425058676,
0.804737854124365,0.696923425058676,0.804737854124365,0.696923425058676,
0.804737854124365,0.696923425058676,0.804737854124365,0.696923425058676,
0.804737854124365,0.696923425058676,0.804737854124365,0.696923425058676,
0.804737854124365,0.696923425058676,0.804737854124365,0.696923425058676,
0.804737854124365,0.696923425058676,0.804737854124365,0.696923425058676,
0.804737854124365,0.696923425058676,0.804737854124365,0.696923425058676,
0.804737854124365,0.696923425058676,0.804737854124365,0.696923425058676,
0.804737854124365,0.696923425058676,0.804737854124365,0.696923425058676,
0.804737854124365,0.696923425058676,0.804737854124365,0.696923425058676,
0.804737854124365,0.696923425058676,0.804737854124365,0.696923425058676,
0.804737854124365,0.696923425058676,0.804737854124365,0.696923425058676,
0.804737854124365,0.696923425058676,0.804737854124365,0.696923425058676,
0.804737854124365,0.696923425058676,0.804737854124365,0.696923425058676,
0.804737854124365,0.696923425058676,0.804737854124365,0.696923425058676,
0.804737854124365,0.696923425058676,0.804737854124365,0.696923425058676,
0.804737854124365,0.696923425058676,0.804737854124365,0.696923425058676,
0.804737854124365,0.696923425058676,0.804737854124365,0.696923425058676,
0.804737854124365,0.696923425058676,0.804737854124365),(0.804737854124365,
0.696923425058676,0.804737854124365,0.696923425058676,0.804737854124365,
0.696923425058676,0.804737854124365,0.696923425058676,0.804737854124365,
0.696923425058676,0.804737854124365,0.696923425058676,0.804737854124365,
0.696923425058676,0.804737854124365,0.696923425058676,0.804737854124365,
0.696923425058676,0.804737854124365,0.696923425058676,0.804737854124365,
0.696923425058676,0.804737854124365,0.696923425058676,0.804737854124365,
0.696923425058676,0.804737854124365,0.696923425058676,0.804737854124365,
0.696923425058676,0.804737854124365,0.696923425058676,0.804737854124365,
0.696923425058676,0.804737854124365,0.696923425058676,0.804737854124365,
0.696923425058676,0.804737854124365,0.696923425058676,0.804737854124365,
0.696923425058676,0.804737854124365,0.696923425058676,0.804737854124365,
0.696923425058676,0.804737854124365,0.696923425058676,0.804737854124365,
0.696923425058676,0.804737854124365,0.696923425058676,0.804737854124365,
0.696923425058676,0.804737854124365,0.696923425058676,0.804737854124365,
0.696923425058676,0.804737854124365,0.696923425058676,0.804737854124365,
0.696923425058676,0.804737854124365,0.696923425058676,0.804737854124365,
0.696923425058676,0.804737854124365,0.696923425058676,0.804737854124365,
0.696923425058676,0.804737854124365,0.696923425058676,0.804737854124365),
(1.,0.866025403784439,1.,0.866025403784439,1.,0.866025403784439,1.,0.866025403784439,
1.,0.866025403784439,1.,0.866025403784439,1.,0.866025403784439,1.,0.866025403784439,
1.,0.866025403784439,1.,0.866025403784439,1.,0.866025403784439,1.,0.866025403784439,
1.,0.866025403784439,1.,0.866025403784439,1.,0.866025403784439,1.,0.866025403784439,
1.,0.866025403784439,1.,0.866025403784439,1.,0.866025403784439,1.,0.866025403784439,
1.,0.866025403784439,1.,0.866025403784439,1.,0.866025403784439,1.,0.866025403784439,
1.,0.866025403784439,1.,0.866025403784439,1.,0.866025403784439,1.,0.866025403784439,
1.,0.866025403784439,1.,0.866025403784439,1.,0.866025403784439,1.,0.866025403784439,
1.,0.866025403784439,1.,0.866025403784439,1.,0.866025403784439,1.,0.866025403784439,
1.)))
REPRESENTATION_ITEM('')
SURFACE()
);
#432=(
BOUNDED_SURFACE()
B_SPLINE_SURFACE(3,2,((#18559,#18560,#18561,#18562,#18563,#18564,#18565,
#18566,#18567,#18568,#18569,#18570,#18571,#18572,#18573,#18574,#18575,#18576,
#18577,#18578,#18579,#18580,#18581,#18582,#18583,#18584,#18585,#18586,#18587,
#18588,#18589,#18590,#18591,#18592,#18593,#18594,#18595,#18596,#18597,#18598,
#18599,#18600,#18601,#18602,#18603,#18604,#18605,#18606,#18607,#18608,#18609,
#18610,#18611,#18612,#18613,#18614,#18615,#18616,#18617,#18618,#18619,#18620,
#18621,#18622,#18623,#18624,#18625,#18626,#18627,#18628,#18629,#18630,#18631),
(#18632,#18633,#18634,#18635,#18636,#18637,#18638,#18639,#18640,#18641,
#18642,#18643,#18644,#18645,#18646,#18647,#18648,#18649,#18650,#18651,#18652,
#18653,#18654,#18655,#18656,#18657,#18658,#18659,#18660,#18661,#18662,#18663,
#18664,#18665,#18666,#18667,#18668,#18669,#18670,#18671,#18672,#18673,#18674,
#18675,#18676,#18677,#18678,#18679,#18680,#18681,#18682,#18683,#18684,#18685,
#18686,#18687,#18688,#18689,#18690,#18691,#18692,#18693,#18694,#18695,#18696,
#18697,#18698,#18699,#18700,#18701,#18702,#18703,#18704),(#18705,#18706,
#18707,#18708,#18709,#18710,#18711,#18712,#18713,#18714,#18715,#18716,#18717,
#18718,#18719,#18720,#18721,#18722,#18723,#18724,#18725,#18726,#18727,#18728,
#18729,#18730,#18731,#18732,#18733,#18734,#18735,#18736,#18737,#18738,#18739,
#18740,#18741,#18742,#18743,#18744,#18745,#18746,#18747,#18748,#18749,#18750,
#18751,#18752,#18753,#18754,#18755,#18756,#18757,#18758,#18759,#18760,#18761,
#18762,#18763,#18764,#18765,#18766,#18767,#18768,#18769,#18770,#18771,#18772,
#18773,#18774,#18775,#18776,#18777),(#18778,#18779,#18780,#18781,#18782,
#18783,#18784,#18785,#18786,#18787,#18788,#18789,#18790,#18791,#18792,#18793,
#18794,#18795,#18796,#18797,#18798,#18799,#18800,#18801,#18802,#18803,#18804,
#18805,#18806,#18807,#18808,#18809,#18810,#18811,#18812,#18813,#18814,#18815,
#18816,#18817,#18818,#18819,#18820,#18821,#18822,#18823,#18824,#18825,#18826,
#18827,#18828,#18829,#18830,#18831,#18832,#18833,#18834,#18835,#18836,#18837,
#18838,#18839,#18840,#18841,#18842,#18843,#18844,#18845,#18846,#18847,#18848,
#18849,#18850)),.UNSPECIFIED.,.F.,.F.,.F.)
B_SPLINE_SURFACE_WITH_KNOTS((4,4),(3,2,2,2,2,2,2,2,2,2,2,2,2,2,2,2,2,2,
2,2,2,2,2,2,2,2,2,2,2,2,2,2,2,2,2,2,3),(0.,1.),(0.,0.0277777777777778,0.0555555555555556,
0.0833333333333333,0.111111111111111,0.138888888888889,0.166666666666667,
0.194444444444444,0.222222222222222,0.25,0.277777777777778,0.305555555555556,
0.333333333333333,0.361111111111111,0.388888888888889,0.416666666666667,
0.444444444444444,0.472222222222222,0.5,0.527777777777778,0.555555555555556,
0.583333333333333,0.611111111111111,0.638888888888889,0.666666666666667,
0.694444444444444,0.722222222222222,0.75,0.777777777777778,0.805555555555556,
0.833333333333333,0.861111111111111,0.888888888888889,0.916666666666667,
0.944444444444444,0.972222222222222,1.),.UNSPECIFIED.)
GEOMETRIC_REPRESENTATION_ITEM()
RATIONAL_B_SPLINE_SURFACE(((1.,0.866025403784439,1.,0.866025403784439,1.,
0.866025403784439,1.,0.866025403784439,1.,0.866025403784439,1.,0.866025403784439,
1.,0.866025403784439,1.,0.866025403784439,1.,0.866025403784439,1.,0.866025403784439,
1.,0.866025403784439,1.,0.866025403784439,1.,0.866025403784439,1.,0.866025403784439,
1.,0.866025403784439,1.,0.866025403784439,1.,0.866025403784439,1.,0.866025403784439,
1.,0.866025403784439,1.,0.866025403784439,1.,0.866025403784439,1.,0.866025403784439,
1.,0.866025403784439,1.,0.866025403784439,1.,0.866025403784439,1.,0.866025403784439,
1.,0.866025403784439,1.,0.866025403784439,1.,0.866025403784439,1.,0.866025403784439,
1.,0.866025403784439,1.,0.866025403784439,1.,0.866025403784439,1.,0.866025403784439,
1.,0.866025403784439,1.,0.866025403784439,1.),(0.804737854124365,0.696923425058676,
0.804737854124365,0.696923425058676,0.804737854124365,0.696923425058676,
0.804737854124365,0.696923425058676,0.804737854124365,0.696923425058676,
0.804737854124365,0.696923425058676,0.804737854124365,0.696923425058676,
0.804737854124365,0.696923425058676,0.804737854124365,0.696923425058676,
0.804737854124365,0.696923425058676,0.804737854124365,0.696923425058676,
0.804737854124365,0.696923425058676,0.804737854124365,0.696923425058676,
0.804737854124365,0.696923425058676,0.804737854124365,0.696923425058676,
0.804737854124365,0.696923425058676,0.804737854124365,0.696923425058676,
0.804737854124365,0.696923425058676,0.804737854124365,0.696923425058676,
0.804737854124365,0.696923425058676,0.804737854124365,0.696923425058676,
0.804737854124365,0.696923425058676,0.804737854124365,0.696923425058676,
0.804737854124365,0.696923425058676,0.804737854124365,0.696923425058676,
0.804737854124365,0.696923425058676,0.804737854124365,0.696923425058676,
0.804737854124365,0.696923425058676,0.804737854124365,0.696923425058676,
0.804737854124365,0.696923425058676,0.804737854124365,0.696923425058676,
0.804737854124365,0.696923425058676,0.804737854124365,0.696923425058676,
0.804737854124365,0.696923425058676,0.804737854124365,0.696923425058676,
0.804737854124365,0.696923425058676,0.804737854124365),(0.804737854124365,
0.696923425058676,0.804737854124365,0.696923425058676,0.804737854124365,
0.696923425058676,0.804737854124365,0.696923425058676,0.804737854124365,
0.696923425058676,0.804737854124365,0.696923425058676,0.804737854124365,
0.696923425058676,0.804737854124365,0.696923425058676,0.804737854124365,
0.696923425058676,0.804737854124365,0.696923425058676,0.804737854124365,
0.696923425058676,0.804737854124365,0.696923425058676,0.804737854124365,
0.696923425058676,0.804737854124365,0.696923425058676,0.804737854124365,
0.696923425058676,0.804737854124365,0.696923425058676,0.804737854124365,
0.696923425058676,0.804737854124365,0.696923425058676,0.804737854124365,
0.696923425058676,0.804737854124365,0.696923425058676,0.804737854124365,
0.696923425058676,0.804737854124365,0.696923425058676,0.804737854124365,
0.696923425058676,0.804737854124365,0.696923425058676,0.804737854124365,
0.696923425058676,0.804737854124365,0.696923425058676,0.804737854124365,
0.696923425058676,0.804737854124365,0.696923425058676,0.804737854124365,
0.696923425058676,0.804737854124365,0.696923425058676,0.804737854124365,
0.696923425058676,0.804737854124365,0.696923425058676,0.804737854124365,
0.696923425058676,0.804737854124365,0.696923425058676,0.804737854124365,
0.696923425058676,0.804737854124365,0.696923425058676,0.804737854124365),
(1.,0.866025403784439,1.,0.866025403784439,1.,0.866025403784439,1.,0.866025403784439,
1.,0.866025403784439,1.,0.866025403784439,1.,0.866025403784439,1.,0.866025403784439,
1.,0.866025403784439,1.,0.866025403784439,1.,0.866025403784439,1.,0.866025403784439,
1.,0.866025403784439,1.,0.866025403784439,1.,0.866025403784439,1.,0.866025403784439,
1.,0.866025403784439,1.,0.866025403784439,1.,0.866025403784439,1.,0.866025403784439,
1.,0.866025403784439,1.,0.866025403784439,1.,0.866025403784439,1.,0.866025403784439,
1.,0.866025403784439,1.,0.866025403784439,1.,0.866025403784439,1.,0.866025403784439,
1.,0.866025403784439,1.,0.866025403784439,1.,0.866025403784439,1.,0.866025403784439,
1.,0.866025403784439,1.,0.866025403784439,1.,0.866025403784439,1.,0.866025403784439,
1.)))
REPRESENTATION_ITEM('')
SURFACE()
);
#433=(
BOUNDED_SURFACE()
B_SPLINE_SURFACE(3,2,((#18928,#18929,#18930,#18931,#18932,#18933,#18934,
#18935,#18936,#18937,#18938,#18939,#18940,#18941,#18942,#18943,#18944,#18945,
#18946,#18947,#18948,#18949,#18950,#18951,#18952,#18953,#18954,#18955,#18956,
#18957,#18958,#18959,#18960,#18961,#18962,#18963,#18964,#18965,#18966,#18967,
#18968,#18969,#18970,#18971,#18972,#18973,#18974,#18975,#18976,#18977,#18978,
#18979,#18980,#18981,#18982,#18983,#18984,#18985,#18986,#18987,#18988,#18989,
#18990,#18991,#18992,#18993,#18994,#18995,#18996,#18997,#18998,#18999,#19000),
(#19001,#19002,#19003,#19004,#19005,#19006,#19007,#19008,#19009,#19010,
#19011,#19012,#19013,#19014,#19015,#19016,#19017,#19018,#19019,#19020,#19021,
#19022,#19023,#19024,#19025,#19026,#19027,#19028,#19029,#19030,#19031,#19032,
#19033,#19034,#19035,#19036,#19037,#19038,#19039,#19040,#19041,#19042,#19043,
#19044,#19045,#19046,#19047,#19048,#19049,#19050,#19051,#19052,#19053,#19054,
#19055,#19056,#19057,#19058,#19059,#19060,#19061,#19062,#19063,#19064,#19065,
#19066,#19067,#19068,#19069,#19070,#19071,#19072,#19073),(#19074,#19075,
#19076,#19077,#19078,#19079,#19080,#19081,#19082,#19083,#19084,#19085,#19086,
#19087,#19088,#19089,#19090,#19091,#19092,#19093,#19094,#19095,#19096,#19097,
#19098,#19099,#19100,#19101,#19102,#19103,#19104,#19105,#19106,#19107,#19108,
#19109,#19110,#19111,#19112,#19113,#19114,#19115,#19116,#19117,#19118,#19119,
#19120,#19121,#19122,#19123,#19124,#19125,#19126,#19127,#19128,#19129,#19130,
#19131,#19132,#19133,#19134,#19135,#19136,#19137,#19138,#19139,#19140,#19141,
#19142,#19143,#19144,#19145,#19146),(#19147,#19148,#19149,#19150,#19151,
#19152,#19153,#19154,#19155,#19156,#19157,#19158,#19159,#19160,#19161,#19162,
#19163,#19164,#19165,#19166,#19167,#19168,#19169,#19170,#19171,#19172,#19173,
#19174,#19175,#19176,#19177,#19178,#19179,#19180,#19181,#19182,#19183,#19184,
#19185,#19186,#19187,#19188,#19189,#19190,#19191,#19192,#19193,#19194,#19195,
#19196,#19197,#19198,#19199,#19200,#19201,#19202,#19203,#19204,#19205,#19206,
#19207,#19208,#19209,#19210,#19211,#19212,#19213,#19214,#19215,#19216,#19217,
#19218,#19219)),.UNSPECIFIED.,.F.,.F.,.F.)
B_SPLINE_SURFACE_WITH_KNOTS((4,4),(3,2,2,2,2,2,2,2,2,2,2,2,2,2,2,2,2,2,
2,2,2,2,2,2,2,2,2,2,2,2,2,2,2,2,2,2,3),(0.,1.),(0.,0.0277777777777778,0.0555555555555556,
0.0833333333333333,0.111111111111111,0.138888888888889,0.166666666666667,
0.194444444444444,0.222222222222222,0.25,0.277777777777778,0.305555555555556,
0.333333333333333,0.361111111111111,0.388888888888889,0.416666666666667,
0.444444444444444,0.472222222222222,0.5,0.527777777777778,0.555555555555556,
0.583333333333333,0.611111111111111,0.638888888888889,0.666666666666667,
0.694444444444444,0.722222222222222,0.75,0.777777777777778,0.805555555555556,
0.833333333333333,0.861111111111111,0.888888888888889,0.916666666666667,
0.944444444444444,0.972222222222222,1.),.UNSPECIFIED.)
GEOMETRIC_REPRESENTATION_ITEM()
RATIONAL_B_SPLINE_SURFACE(((1.,0.866025403784439,1.,0.866025403784439,1.,
0.866025403784439,1.,0.866025403784439,1.,0.866025403784439,1.,0.866025403784439,
1.,0.866025403784439,1.,0.866025403784439,1.,0.866025403784439,1.,0.866025403784439,
1.,0.866025403784439,1.,0.866025403784439,1.,0.866025403784439,1.,0.866025403784439,
1.,0.866025403784439,1.,0.866025403784439,1.,0.866025403784439,1.,0.866025403784439,
1.,0.866025403784439,1.,0.866025403784439,1.,0.866025403784439,1.,0.866025403784439,
1.,0.866025403784439,1.,0.866025403784439,1.,0.866025403784439,1.,0.866025403784439,
1.,0.866025403784439,1.,0.866025403784439,1.,0.866025403784439,1.,0.866025403784439,
1.,0.866025403784439,1.,0.866025403784439,1.,0.866025403784439,1.,0.866025403784439,
1.,0.866025403784439,1.,0.866025403784439,1.),(0.804737854124365,0.696923425058676,
0.804737854124365,0.696923425058676,0.804737854124365,0.696923425058676,
0.804737854124365,0.696923425058676,0.804737854124365,0.696923425058676,
0.804737854124365,0.696923425058676,0.804737854124365,0.696923425058676,
0.804737854124365,0.696923425058676,0.804737854124365,0.696923425058676,
0.804737854124365,0.696923425058676,0.804737854124365,0.696923425058676,
0.804737854124365,0.696923425058676,0.804737854124365,0.696923425058676,
0.804737854124365,0.696923425058676,0.804737854124365,0.696923425058676,
0.804737854124365,0.696923425058676,0.804737854124365,0.696923425058676,
0.804737854124365,0.696923425058676,0.804737854124365,0.696923425058676,
0.804737854124365,0.696923425058676,0.804737854124365,0.696923425058676,
0.804737854124365,0.696923425058676,0.804737854124365,0.696923425058676,
0.804737854124365,0.696923425058676,0.804737854124365,0.696923425058676,
0.804737854124365,0.696923425058676,0.804737854124365,0.696923425058676,
0.804737854124365,0.696923425058676,0.804737854124365,0.696923425058676,
0.804737854124365,0.696923425058676,0.804737854124365,0.696923425058676,
0.804737854124365,0.696923425058676,0.804737854124365,0.696923425058676,
0.804737854124365,0.696923425058676,0.804737854124365,0.696923425058676,
0.804737854124365,0.696923425058676,0.804737854124365),(0.804737854124365,
0.696923425058676,0.804737854124365,0.696923425058676,0.804737854124365,
0.696923425058676,0.804737854124365,0.696923425058676,0.804737854124365,
0.696923425058676,0.804737854124365,0.696923425058676,0.804737854124365,
0.696923425058676,0.804737854124365,0.696923425058676,0.804737854124365,
0.696923425058676,0.804737854124365,0.696923425058676,0.804737854124365,
0.696923425058676,0.804737854124365,0.696923425058676,0.804737854124365,
0.696923425058676,0.804737854124365,0.696923425058676,0.804737854124365,
0.696923425058676,0.804737854124365,0.696923425058676,0.804737854124365,
0.696923425058676,0.804737854124365,0.696923425058676,0.804737854124365,
0.696923425058676,0.804737854124365,0.696923425058676,0.804737854124365,
0.696923425058676,0.804737854124365,0.696923425058676,0.804737854124365,
0.696923425058676,0.804737854124365,0.696923425058676,0.804737854124365,
0.696923425058676,0.804737854124365,0.696923425058676,0.804737854124365,
0.696923425058676,0.804737854124365,0.696923425058676,0.804737854124365,
0.696923425058676,0.804737854124365,0.696923425058676,0.804737854124365,
0.696923425058676,0.804737854124365,0.696923425058676,0.804737854124365,
0.696923425058676,0.804737854124365,0.696923425058676,0.804737854124365,
0.696923425058676,0.804737854124365,0.696923425058676,0.804737854124365),
(1.,0.866025403784439,1.,0.866025403784439,1.,0.866025403784439,1.,0.866025403784439,
1.,0.866025403784439,1.,0.866025403784439,1.,0.866025403784439,1.,0.866025403784439,
1.,0.866025403784439,1.,0.866025403784439,1.,0.866025403784439,1.,0.866025403784439,
1.,0.866025403784439,1.,0.866025403784439,1.,0.866025403784439,1.,0.866025403784439,
1.,0.866025403784439,1.,0.866025403784439,1.,0.866025403784439,1.,0.866025403784439,
1.,0.866025403784439,1.,0.866025403784439,1.,0.866025403784439,1.,0.866025403784439,
1.,0.866025403784439,1.,0.866025403784439,1.,0.866025403784439,1.,0.866025403784439,
1.,0.866025403784439,1.,0.866025403784439,1.,0.866025403784439,1.,0.866025403784439,
1.,0.866025403784439,1.,0.866025403784439,1.,0.866025403784439,1.,0.866025403784439,
1.)))
REPRESENTATION_ITEM('')
SURFACE()
);
#434=(
BOUNDED_SURFACE()
B_SPLINE_SURFACE(3,2,((#19297,#19298,#19299,#19300,#19301,#19302,#19303,
#19304,#19305,#19306,#19307,#19308,#19309,#19310,#19311,#19312,#19313,#19314,
#19315,#19316,#19317,#19318,#19319,#19320,#19321,#19322,#19323,#19324,#19325,
#19326,#19327,#19328,#19329,#19330,#19331,#19332,#19333,#19334,#19335,#19336,
#19337,#19338,#19339,#19340,#19341,#19342,#19343,#19344,#19345,#19346,#19347,
#19348,#19349,#19350,#19351,#19352,#19353,#19354,#19355,#19356,#19357,#19358,
#19359,#19360,#19361,#19362,#19363,#19364,#19365,#19366,#19367,#19368,#19369),
(#19370,#19371,#19372,#19373,#19374,#19375,#19376,#19377,#19378,#19379,
#19380,#19381,#19382,#19383,#19384,#19385,#19386,#19387,#19388,#19389,#19390,
#19391,#19392,#19393,#19394,#19395,#19396,#19397,#19398,#19399,#19400,#19401,
#19402,#19403,#19404,#19405,#19406,#19407,#19408,#19409,#19410,#19411,#19412,
#19413,#19414,#19415,#19416,#19417,#19418,#19419,#19420,#19421,#19422,#19423,
#19424,#19425,#19426,#19427,#19428,#19429,#19430,#19431,#19432,#19433,#19434,
#19435,#19436,#19437,#19438,#19439,#19440,#19441,#19442),(#19443,#19444,
#19445,#19446,#19447,#19448,#19449,#19450,#19451,#19452,#19453,#19454,#19455,
#19456,#19457,#19458,#19459,#19460,#19461,#19462,#19463,#19464,#19465,#19466,
#19467,#19468,#19469,#19470,#19471,#19472,#19473,#19474,#19475,#19476,#19477,
#19478,#19479,#19480,#19481,#19482,#19483,#19484,#19485,#19486,#19487,#19488,
#19489,#19490,#19491,#19492,#19493,#19494,#19495,#19496,#19497,#19498,#19499,
#19500,#19501,#19502,#19503,#19504,#19505,#19506,#19507,#19508,#19509,#19510,
#19511,#19512,#19513,#19514,#19515),(#19516,#19517,#19518,#19519,#19520,
#19521,#19522,#19523,#19524,#19525,#19526,#19527,#19528,#19529,#19530,#19531,
#19532,#19533,#19534,#19535,#19536,#19537,#19538,#19539,#19540,#19541,#19542,
#19543,#19544,#19545,#19546,#19547,#19548,#19549,#19550,#19551,#19552,#19553,
#19554,#19555,#19556,#19557,#19558,#19559,#19560,#19561,#19562,#19563,#19564,
#19565,#19566,#19567,#19568,#19569,#19570,#19571,#19572,#19573,#19574,#19575,
#19576,#19577,#19578,#19579,#19580,#19581,#19582,#19583,#19584,#19585,#19586,
#19587,#19588)),.UNSPECIFIED.,.F.,.F.,.F.)
B_SPLINE_SURFACE_WITH_KNOTS((4,4),(3,2,2,2,2,2,2,2,2,2,2,2,2,2,2,2,2,2,
2,2,2,2,2,2,2,2,2,2,2,2,2,2,2,2,2,2,3),(0.,1.),(0.,0.0277777777777778,0.0555555555555556,
0.0833333333333333,0.111111111111111,0.138888888888889,0.166666666666667,
0.194444444444444,0.222222222222222,0.25,0.277777777777778,0.305555555555556,
0.333333333333333,0.361111111111111,0.388888888888889,0.416666666666667,
0.444444444444444,0.472222222222222,0.5,0.527777777777778,0.555555555555556,
0.583333333333333,0.611111111111111,0.638888888888889,0.666666666666667,
0.694444444444444,0.722222222222222,0.75,0.777777777777778,0.805555555555556,
0.833333333333333,0.861111111111111,0.888888888888889,0.916666666666667,
0.944444444444444,0.972222222222222,1.),.UNSPECIFIED.)
GEOMETRIC_REPRESENTATION_ITEM()
RATIONAL_B_SPLINE_SURFACE(((1.,0.866025403784439,1.,0.866025403784439,1.,
0.866025403784439,1.,0.866025403784439,1.,0.866025403784439,1.,0.866025403784439,
1.,0.866025403784439,1.,0.866025403784439,1.,0.866025403784439,1.,0.866025403784439,
1.,0.866025403784439,1.,0.866025403784439,1.,0.866025403784439,1.,0.866025403784439,
1.,0.866025403784439,1.,0.866025403784439,1.,0.866025403784439,1.,0.866025403784439,
1.,0.866025403784439,1.,0.866025403784439,1.,0.866025403784439,1.,0.866025403784439,
1.,0.866025403784439,1.,0.866025403784439,1.,0.866025403784439,1.,0.866025403784439,
1.,0.866025403784439,1.,0.866025403784439,1.,0.866025403784439,1.,0.866025403784439,
1.,0.866025403784439,1.,0.866025403784439,1.,0.866025403784439,1.,0.866025403784439,
1.,0.866025403784439,1.,0.866025403784439,1.),(0.804737854124365,0.696923425058676,
0.804737854124365,0.696923425058676,0.804737854124365,0.696923425058676,
0.804737854124365,0.696923425058676,0.804737854124365,0.696923425058676,
0.804737854124365,0.696923425058676,0.804737854124365,0.696923425058676,
0.804737854124365,0.696923425058676,0.804737854124365,0.696923425058676,
0.804737854124365,0.696923425058676,0.804737854124365,0.696923425058676,
0.804737854124365,0.696923425058676,0.804737854124365,0.696923425058676,
0.804737854124365,0.696923425058676,0.804737854124365,0.696923425058676,
0.804737854124365,0.696923425058676,0.804737854124365,0.696923425058676,
0.804737854124365,0.696923425058676,0.804737854124365,0.696923425058676,
0.804737854124365,0.696923425058676,0.804737854124365,0.696923425058676,
0.804737854124365,0.696923425058676,0.804737854124365,0.696923425058676,
0.804737854124365,0.696923425058676,0.804737854124365,0.696923425058676,
0.804737854124365,0.696923425058676,0.804737854124365,0.696923425058676,
0.804737854124365,0.696923425058676,0.804737854124365,0.696923425058676,
0.804737854124365,0.696923425058676,0.804737854124365,0.696923425058676,
0.804737854124365,0.696923425058676,0.804737854124365,0.696923425058676,
0.804737854124365,0.696923425058676,0.804737854124365,0.696923425058676,
0.804737854124365,0.696923425058676,0.804737854124365),(0.804737854124365,
0.696923425058676,0.804737854124365,0.696923425058676,0.804737854124365,
0.696923425058676,0.804737854124365,0.696923425058676,0.804737854124365,
0.696923425058676,0.804737854124365,0.696923425058676,0.804737854124365,
0.696923425058676,0.804737854124365,0.696923425058676,0.804737854124365,
0.696923425058676,0.804737854124365,0.696923425058676,0.804737854124365,
0.696923425058676,0.804737854124365,0.696923425058676,0.804737854124365,
0.696923425058676,0.804737854124365,0.696923425058676,0.804737854124365,
0.696923425058676,0.804737854124365,0.696923425058676,0.804737854124365,
0.696923425058676,0.804737854124365,0.696923425058676,0.804737854124365,
0.696923425058676,0.804737854124365,0.696923425058676,0.804737854124365,
0.696923425058676,0.804737854124365,0.696923425058676,0.804737854124365,
0.696923425058676,0.804737854124365,0.696923425058676,0.804737854124365,
0.696923425058676,0.804737854124365,0.696923425058676,0.804737854124365,
0.696923425058676,0.804737854124365,0.696923425058676,0.804737854124365,
0.696923425058676,0.804737854124365,0.696923425058676,0.804737854124365,
0.696923425058676,0.804737854124365,0.696923425058676,0.804737854124365,
0.696923425058676,0.804737854124365,0.696923425058676,0.804737854124365,
0.696923425058676,0.804737854124365,0.696923425058676,0.804737854124365),
(1.,0.866025403784439,1.,0.866025403784439,1.,0.866025403784439,1.,0.866025403784439,
1.,0.866025403784439,1.,0.866025403784439,1.,0.866025403784439,1.,0.866025403784439,
1.,0.866025403784439,1.,0.866025403784439,1.,0.866025403784439,1.,0.866025403784439,
1.,0.866025403784439,1.,0.866025403784439,1.,0.866025403784439,1.,0.866025403784439,
1.,0.866025403784439,1.,0.866025403784439,1.,0.866025403784439,1.,0.866025403784439,
1.,0.866025403784439,1.,0.866025403784439,1.,0.866025403784439,1.,0.866025403784439,
1.,0.866025403784439,1.,0.866025403784439,1.,0.866025403784439,1.,0.866025403784439,
1.,0.866025403784439,1.,0.866025403784439,1.,0.866025403784439,1.,0.866025403784439,
1.,0.866025403784439,1.,0.866025403784439,1.,0.866025403784439,1.,0.866025403784439,
1.)))
REPRESENTATION_ITEM('')
SURFACE()
);
#435=(
BOUNDED_SURFACE()
B_SPLINE_SURFACE(3,2,((#19594,#19595,#19596,#19597,#19598,#19599,#19600,
#19601,#19602,#19603,#19604,#19605,#19606,#19607,#19608,#19609,#19610,#19611,
#19612,#19613,#19614,#19615,#19616,#19617,#19618,#19619,#19620,#19621,#19622,
#19623,#19624,#19625,#19626,#19627,#19628,#19629,#19630,#19631,#19632,#19633,
#19634,#19635,#19636,#19637,#19638,#19639,#19640,#19641,#19642,#19643,#19644,
#19645,#19646,#19647,#19648,#19649,#19650,#19651,#19652,#19653,#19654,#19655,
#19656,#19657,#19658,#19659,#19660,#19661,#19662,#19663,#19664,#19665,#19666),
(#19667,#19668,#19669,#19670,#19671,#19672,#19673,#19674,#19675,#19676,
#19677,#19678,#19679,#19680,#19681,#19682,#19683,#19684,#19685,#19686,#19687,
#19688,#19689,#19690,#19691,#19692,#19693,#19694,#19695,#19696,#19697,#19698,
#19699,#19700,#19701,#19702,#19703,#19704,#19705,#19706,#19707,#19708,#19709,
#19710,#19711,#19712,#19713,#19714,#19715,#19716,#19717,#19718,#19719,#19720,
#19721,#19722,#19723,#19724,#19725,#19726,#19727,#19728,#19729,#19730,#19731,
#19732,#19733,#19734,#19735,#19736,#19737,#19738,#19739),(#19740,#19741,
#19742,#19743,#19744,#19745,#19746,#19747,#19748,#19749,#19750,#19751,#19752,
#19753,#19754,#19755,#19756,#19757,#19758,#19759,#19760,#19761,#19762,#19763,
#19764,#19765,#19766,#19767,#19768,#19769,#19770,#19771,#19772,#19773,#19774,
#19775,#19776,#19777,#19778,#19779,#19780,#19781,#19782,#19783,#19784,#19785,
#19786,#19787,#19788,#19789,#19790,#19791,#19792,#19793,#19794,#19795,#19796,
#19797,#19798,#19799,#19800,#19801,#19802,#19803,#19804,#19805,#19806,#19807,
#19808,#19809,#19810,#19811,#19812),(#19813,#19814,#19815,#19816,#19817,
#19818,#19819,#19820,#19821,#19822,#19823,#19824,#19825,#19826,#19827,#19828,
#19829,#19830,#19831,#19832,#19833,#19834,#19835,#19836,#19837,#19838,#19839,
#19840,#19841,#19842,#19843,#19844,#19845,#19846,#19847,#19848,#19849,#19850,
#19851,#19852,#19853,#19854,#19855,#19856,#19857,#19858,#19859,#19860,#19861,
#19862,#19863,#19864,#19865,#19866,#19867,#19868,#19869,#19870,#19871,#19872,
#19873,#19874,#19875,#19876,#19877,#19878,#19879,#19880,#19881,#19882,#19883,
#19884,#19885)),.UNSPECIFIED.,.F.,.F.,.F.)
B_SPLINE_SURFACE_WITH_KNOTS((4,4),(3,2,2,2,2,2,2,2,2,2,2,2,2,2,2,2,2,2,
2,2,2,2,2,2,2,2,2,2,2,2,2,2,2,2,2,2,3),(0.,1.),(0.,0.0277777777777778,0.0555555555555556,
0.0833333333333333,0.111111111111111,0.138888888888889,0.166666666666667,
0.194444444444444,0.222222222222222,0.25,0.277777777777778,0.305555555555556,
0.333333333333333,0.361111111111111,0.388888888888889,0.416666666666667,
0.444444444444444,0.472222222222222,0.5,0.527777777777778,0.555555555555556,
0.583333333333333,0.611111111111111,0.638888888888889,0.666666666666667,
0.694444444444444,0.722222222222222,0.75,0.777777777777778,0.805555555555556,
0.833333333333333,0.861111111111111,0.888888888888889,0.916666666666667,
0.944444444444444,0.972222222222222,1.),.UNSPECIFIED.)
GEOMETRIC_REPRESENTATION_ITEM()
RATIONAL_B_SPLINE_SURFACE(((1.,0.866025403784439,1.,0.866025403784439,1.,
0.866025403784439,1.,0.866025403784439,1.,0.866025403784439,1.,0.866025403784439,
1.,0.866025403784439,1.,0.866025403784439,1.,0.866025403784439,1.,0.866025403784439,
1.,0.866025403784439,1.,0.866025403784439,1.,0.866025403784439,1.,0.866025403784439,
1.,0.866025403784439,1.,0.866025403784439,1.,0.866025403784439,1.,0.866025403784439,
1.,0.866025403784439,1.,0.866025403784439,1.,0.866025403784439,1.,0.866025403784439,
1.,0.866025403784439,1.,0.866025403784439,1.,0.866025403784439,1.,0.866025403784439,
1.,0.866025403784439,1.,0.866025403784439,1.,0.866025403784439,1.,0.866025403784439,
1.,0.866025403784439,1.,0.866025403784439,1.,0.866025403784439,1.,0.866025403784439,
1.,0.866025403784439,1.,0.866025403784439,1.),(0.804737854124365,0.696923425058676,
0.804737854124365,0.696923425058676,0.804737854124365,0.696923425058676,
0.804737854124365,0.696923425058676,0.804737854124365,0.696923425058676,
0.804737854124365,0.696923425058676,0.804737854124365,0.696923425058676,
0.804737854124365,0.696923425058676,0.804737854124365,0.696923425058676,
0.804737854124365,0.696923425058676,0.804737854124365,0.696923425058676,
0.804737854124365,0.696923425058676,0.804737854124365,0.696923425058676,
0.804737854124365,0.696923425058676,0.804737854124365,0.696923425058676,
0.804737854124365,0.696923425058676,0.804737854124365,0.696923425058676,
0.804737854124365,0.696923425058676,0.804737854124365,0.696923425058676,
0.804737854124365,0.696923425058676,0.804737854124365,0.696923425058676,
0.804737854124365,0.696923425058676,0.804737854124365,0.696923425058676,
0.804737854124365,0.696923425058676,0.804737854124365,0.696923425058676,
0.804737854124365,0.696923425058676,0.804737854124365,0.696923425058676,
0.804737854124365,0.696923425058676,0.804737854124365,0.696923425058676,
0.804737854124365,0.696923425058676,0.804737854124365,0.696923425058676,
0.804737854124365,0.696923425058676,0.804737854124365,0.696923425058676,
0.804737854124365,0.696923425058676,0.804737854124365,0.696923425058676,
0.804737854124365,0.696923425058676,0.804737854124365),(0.804737854124365,
0.696923425058676,0.804737854124365,0.696923425058676,0.804737854124365,
0.696923425058676,0.804737854124365,0.696923425058676,0.804737854124365,
0.696923425058676,0.804737854124365,0.696923425058676,0.804737854124365,
0.696923425058676,0.804737854124365,0.696923425058676,0.804737854124365,
0.696923425058676,0.804737854124365,0.696923425058676,0.804737854124365,
0.696923425058676,0.804737854124365,0.696923425058676,0.804737854124365,
0.696923425058676,0.804737854124365,0.696923425058676,0.804737854124365,
0.696923425058676,0.804737854124365,0.696923425058676,0.804737854124365,
0.696923425058676,0.804737854124365,0.696923425058676,0.804737854124365,
0.696923425058676,0.804737854124365,0.696923425058676,0.804737854124365,
0.696923425058676,0.804737854124365,0.696923425058676,0.804737854124365,
0.696923425058676,0.804737854124365,0.696923425058676,0.804737854124365,
0.696923425058676,0.804737854124365,0.696923425058676,0.804737854124365,
0.696923425058676,0.804737854124365,0.696923425058676,0.804737854124365,
0.696923425058676,0.804737854124365,0.696923425058676,0.804737854124365,
0.696923425058676,0.804737854124365,0.696923425058676,0.804737854124365,
0.696923425058676,0.804737854124365,0.696923425058676,0.804737854124365,
0.696923425058676,0.804737854124365,0.696923425058676,0.804737854124365),
(1.,0.866025403784439,1.,0.866025403784439,1.,0.866025403784439,1.,0.866025403784439,
1.,0.866025403784439,1.,0.866025403784439,1.,0.866025403784439,1.,0.866025403784439,
1.,0.866025403784439,1.,0.866025403784439,1.,0.866025403784439,1.,0.866025403784439,
1.,0.866025403784439,1.,0.866025403784439,1.,0.866025403784439,1.,0.866025403784439,
1.,0.866025403784439,1.,0.866025403784439,1.,0.866025403784439,1.,0.866025403784439,
1.,0.866025403784439,1.,0.866025403784439,1.,0.866025403784439,1.,0.866025403784439,
1.,0.866025403784439,1.,0.866025403784439,1.,0.866025403784439,1.,0.866025403784439,
1.,0.866025403784439,1.,0.866025403784439,1.,0.866025403784439,1.,0.866025403784439,
1.,0.866025403784439,1.,0.866025403784439,1.,0.866025403784439,1.,0.866025403784439,
1.)))
REPRESENTATION_ITEM('')
SURFACE()
);
#436=(
BOUNDED_SURFACE()
B_SPLINE_SURFACE(3,2,((#20040,#20041,#20042,#20043,#20044,#20045,#20046,
#20047,#20048,#20049,#20050,#20051,#20052,#20053,#20054,#20055,#20056,#20057,
#20058,#20059,#20060,#20061,#20062,#20063,#20064,#20065,#20066,#20067,#20068,
#20069,#20070,#20071,#20072,#20073,#20074,#20075,#20076,#20077,#20078,#20079,
#20080,#20081,#20082,#20083,#20084,#20085,#20086,#20087,#20088,#20089,#20090,
#20091,#20092,#20093,#20094,#20095,#20096,#20097,#20098,#20099,#20100,#20101,
#20102,#20103,#20104,#20105,#20106,#20107,#20108,#20109,#20110,#20111,#20112),
(#20113,#20114,#20115,#20116,#20117,#20118,#20119,#20120,#20121,#20122,
#20123,#20124,#20125,#20126,#20127,#20128,#20129,#20130,#20131,#20132,#20133,
#20134,#20135,#20136,#20137,#20138,#20139,#20140,#20141,#20142,#20143,#20144,
#20145,#20146,#20147,#20148,#20149,#20150,#20151,#20152,#20153,#20154,#20155,
#20156,#20157,#20158,#20159,#20160,#20161,#20162,#20163,#20164,#20165,#20166,
#20167,#20168,#20169,#20170,#20171,#20172,#20173,#20174,#20175,#20176,#20177,
#20178,#20179,#20180,#20181,#20182,#20183,#20184,#20185),(#20186,#20187,
#20188,#20189,#20190,#20191,#20192,#20193,#20194,#20195,#20196,#20197,#20198,
#20199,#20200,#20201,#20202,#20203,#20204,#20205,#20206,#20207,#20208,#20209,
#20210,#20211,#20212,#20213,#20214,#20215,#20216,#20217,#20218,#20219,#20220,
#20221,#20222,#20223,#20224,#20225,#20226,#20227,#20228,#20229,#20230,#20231,
#20232,#20233,#20234,#20235,#20236,#20237,#20238,#20239,#20240,#20241,#20242,
#20243,#20244,#20245,#20246,#20247,#20248,#20249,#20250,#20251,#20252,#20253,
#20254,#20255,#20256,#20257,#20258),(#20259,#20260,#20261,#20262,#20263,
#20264,#20265,#20266,#20267,#20268,#20269,#20270,#20271,#20272,#20273,#20274,
#20275,#20276,#20277,#20278,#20279,#20280,#20281,#20282,#20283,#20284,#20285,
#20286,#20287,#20288,#20289,#20290,#20291,#20292,#20293,#20294,#20295,#20296,
#20297,#20298,#20299,#20300,#20301,#20302,#20303,#20304,#20305,#20306,#20307,
#20308,#20309,#20310,#20311,#20312,#20313,#20314,#20315,#20316,#20317,#20318,
#20319,#20320,#20321,#20322,#20323,#20324,#20325,#20326,#20327,#20328,#20329,
#20330,#20331)),.UNSPECIFIED.,.F.,.F.,.F.)
B_SPLINE_SURFACE_WITH_KNOTS((4,4),(3,2,2,2,2,2,2,2,2,2,2,2,2,2,2,2,2,2,
2,2,2,2,2,2,2,2,2,2,2,2,2,2,2,2,2,2,3),(0.,1.),(0.,0.0277777777777778,0.0555555555555556,
0.0833333333333333,0.111111111111111,0.138888888888889,0.166666666666667,
0.194444444444444,0.222222222222222,0.25,0.277777777777778,0.305555555555556,
0.333333333333333,0.361111111111111,0.388888888888889,0.416666666666667,
0.444444444444444,0.472222222222222,0.5,0.527777777777778,0.555555555555556,
0.583333333333333,0.611111111111111,0.638888888888889,0.666666666666667,
0.694444444444444,0.722222222222222,0.75,0.777777777777778,0.805555555555556,
0.833333333333333,0.861111111111111,0.888888888888889,0.916666666666667,
0.944444444444444,0.972222222222222,1.),.UNSPECIFIED.)
GEOMETRIC_REPRESENTATION_ITEM()
RATIONAL_B_SPLINE_SURFACE(((1.,0.866025403784439,1.,0.866025403784439,1.,
0.866025403784439,1.,0.866025403784439,1.,0.866025403784439,1.,0.866025403784439,
1.,0.866025403784439,1.,0.866025403784439,1.,0.866025403784439,1.,0.866025403784439,
1.,0.866025403784439,1.,0.866025403784439,1.,0.866025403784439,1.,0.866025403784439,
1.,0.866025403784439,1.,0.866025403784439,1.,0.866025403784439,1.,0.866025403784439,
1.,0.866025403784439,1.,0.866025403784439,1.,0.866025403784439,1.,0.866025403784439,
1.,0.866025403784439,1.,0.866025403784439,1.,0.866025403784439,1.,0.866025403784439,
1.,0.866025403784439,1.,0.866025403784439,1.,0.866025403784439,1.,0.866025403784439,
1.,0.866025403784439,1.,0.866025403784439,1.,0.866025403784439,1.,0.866025403784439,
1.,0.866025403784439,1.,0.866025403784439,1.),(0.804737854124365,0.696923425058676,
0.804737854124365,0.696923425058676,0.804737854124365,0.696923425058676,
0.804737854124365,0.696923425058676,0.804737854124365,0.696923425058676,
0.804737854124365,0.696923425058676,0.804737854124365,0.696923425058676,
0.804737854124365,0.696923425058676,0.804737854124365,0.696923425058676,
0.804737854124365,0.696923425058676,0.804737854124365,0.696923425058676,
0.804737854124365,0.696923425058676,0.804737854124365,0.696923425058676,
0.804737854124365,0.696923425058676,0.804737854124365,0.696923425058676,
0.804737854124365,0.696923425058676,0.804737854124365,0.696923425058676,
0.804737854124365,0.696923425058676,0.804737854124365,0.696923425058676,
0.804737854124365,0.696923425058676,0.804737854124365,0.696923425058676,
0.804737854124365,0.696923425058676,0.804737854124365,0.696923425058676,
0.804737854124365,0.696923425058676,0.804737854124365,0.696923425058676,
0.804737854124365,0.696923425058676,0.804737854124365,0.696923425058676,
0.804737854124365,0.696923425058676,0.804737854124365,0.696923425058676,
0.804737854124365,0.696923425058676,0.804737854124365,0.696923425058676,
0.804737854124365,0.696923425058676,0.804737854124365,0.696923425058676,
0.804737854124365,0.696923425058676,0.804737854124365,0.696923425058676,
0.804737854124365,0.696923425058676,0.804737854124365),(0.804737854124365,
0.696923425058676,0.804737854124365,0.696923425058676,0.804737854124365,
0.696923425058676,0.804737854124365,0.696923425058676,0.804737854124365,
0.696923425058676,0.804737854124365,0.696923425058676,0.804737854124365,
0.696923425058676,0.804737854124365,0.696923425058676,0.804737854124365,
0.696923425058676,0.804737854124365,0.696923425058676,0.804737854124365,
0.696923425058676,0.804737854124365,0.696923425058676,0.804737854124365,
0.696923425058676,0.804737854124365,0.696923425058676,0.804737854124365,
0.696923425058676,0.804737854124365,0.696923425058676,0.804737854124365,
0.696923425058676,0.804737854124365,0.696923425058676,0.804737854124365,
0.696923425058676,0.804737854124365,0.696923425058676,0.804737854124365,
0.696923425058676,0.804737854124365,0.696923425058676,0.804737854124365,
0.696923425058676,0.804737854124365,0.696923425058676,0.804737854124365,
0.696923425058676,0.804737854124365,0.696923425058676,0.804737854124365,
0.696923425058676,0.804737854124365,0.696923425058676,0.804737854124365,
0.696923425058676,0.804737854124365,0.696923425058676,0.804737854124365,
0.696923425058676,0.804737854124365,0.696923425058676,0.804737854124365,
0.696923425058676,0.804737854124365,0.696923425058676,0.804737854124365,
0.696923425058676,0.804737854124365,0.696923425058676,0.804737854124365),
(1.,0.866025403784439,1.,0.866025403784439,1.,0.866025403784439,1.,0.866025403784439,
1.,0.866025403784439,1.,0.866025403784439,1.,0.866025403784439,1.,0.866025403784439,
1.,0.866025403784439,1.,0.866025403784439,1.,0.866025403784439,1.,0.866025403784439,
1.,0.866025403784439,1.,0.866025403784439,1.,0.866025403784439,1.,0.866025403784439,
1.,0.866025403784439,1.,0.866025403784439,1.,0.866025403784439,1.,0.866025403784439,
1.,0.866025403784439,1.,0.866025403784439,1.,0.866025403784439,1.,0.866025403784439,
1.,0.866025403784439,1.,0.866025403784439,1.,0.866025403784439,1.,0.866025403784439,
1.,0.866025403784439,1.,0.866025403784439,1.,0.866025403784439,1.,0.866025403784439,
1.,0.866025403784439,1.,0.866025403784439,1.,0.866025403784439,1.,0.866025403784439,
1.)))
REPRESENTATION_ITEM('')
SURFACE()
);
#437=(
BOUNDED_SURFACE()
B_SPLINE_SURFACE(3,2,((#20409,#20410,#20411,#20412,#20413,#20414,#20415,
#20416,#20417,#20418,#20419,#20420,#20421,#20422,#20423,#20424,#20425,#20426,
#20427,#20428,#20429,#20430,#20431,#20432,#20433,#20434,#20435,#20436,#20437,
#20438,#20439,#20440,#20441,#20442,#20443,#20444,#20445,#20446,#20447,#20448,
#20449,#20450,#20451,#20452,#20453,#20454,#20455,#20456,#20457,#20458,#20459,
#20460,#20461,#20462,#20463,#20464,#20465,#20466,#20467,#20468,#20469,#20470,
#20471,#20472,#20473,#20474,#20475,#20476,#20477,#20478,#20479,#20480,#20481),
(#20482,#20483,#20484,#20485,#20486,#20487,#20488,#20489,#20490,#20491,
#20492,#20493,#20494,#20495,#20496,#20497,#20498,#20499,#20500,#20501,#20502,
#20503,#20504,#20505,#20506,#20507,#20508,#20509,#20510,#20511,#20512,#20513,
#20514,#20515,#20516,#20517,#20518,#20519,#20520,#20521,#20522,#20523,#20524,
#20525,#20526,#20527,#20528,#20529,#20530,#20531,#20532,#20533,#20534,#20535,
#20536,#20537,#20538,#20539,#20540,#20541,#20542,#20543,#20544,#20545,#20546,
#20547,#20548,#20549,#20550,#20551,#20552,#20553,#20554),(#20555,#20556,
#20557,#20558,#20559,#20560,#20561,#20562,#20563,#20564,#20565,#20566,#20567,
#20568,#20569,#20570,#20571,#20572,#20573,#20574,#20575,#20576,#20577,#20578,
#20579,#20580,#20581,#20582,#20583,#20584,#20585,#20586,#20587,#20588,#20589,
#20590,#20591,#20592,#20593,#20594,#20595,#20596,#20597,#20598,#20599,#20600,
#20601,#20602,#20603,#20604,#20605,#20606,#20607,#20608,#20609,#20610,#20611,
#20612,#20613,#20614,#20615,#20616,#20617,#20618,#20619,#20620,#20621,#20622,
#20623,#20624,#20625,#20626,#20627),(#20628,#20629,#20630,#20631,#20632,
#20633,#20634,#20635,#20636,#20637,#20638,#20639,#20640,#20641,#20642,#20643,
#20644,#20645,#20646,#20647,#20648,#20649,#20650,#20651,#20652,#20653,#20654,
#20655,#20656,#20657,#20658,#20659,#20660,#20661,#20662,#20663,#20664,#20665,
#20666,#20667,#20668,#20669,#20670,#20671,#20672,#20673,#20674,#20675,#20676,
#20677,#20678,#20679,#20680,#20681,#20682,#20683,#20684,#20685,#20686,#20687,
#20688,#20689,#20690,#20691,#20692,#20693,#20694,#20695,#20696,#20697,#20698,
#20699,#20700)),.UNSPECIFIED.,.F.,.F.,.F.)
B_SPLINE_SURFACE_WITH_KNOTS((4,4),(3,2,2,2,2,2,2,2,2,2,2,2,2,2,2,2,2,2,
2,2,2,2,2,2,2,2,2,2,2,2,2,2,2,2,2,2,3),(0.,1.),(0.,0.0277777777777778,0.0555555555555556,
0.0833333333333333,0.111111111111111,0.138888888888889,0.166666666666667,
0.194444444444444,0.222222222222222,0.25,0.277777777777778,0.305555555555556,
0.333333333333333,0.361111111111111,0.388888888888889,0.416666666666667,
0.444444444444444,0.472222222222222,0.5,0.527777777777778,0.555555555555556,
0.583333333333333,0.611111111111111,0.638888888888889,0.666666666666667,
0.694444444444444,0.722222222222222,0.75,0.777777777777778,0.805555555555556,
0.833333333333333,0.861111111111111,0.888888888888889,0.916666666666667,
0.944444444444444,0.972222222222222,1.),.UNSPECIFIED.)
GEOMETRIC_REPRESENTATION_ITEM()
RATIONAL_B_SPLINE_SURFACE(((1.,0.866025403784439,1.,0.866025403784439,1.,
0.866025403784439,1.,0.866025403784439,1.,0.866025403784439,1.,0.866025403784439,
1.,0.866025403784439,1.,0.866025403784439,1.,0.866025403784439,1.,0.866025403784439,
1.,0.866025403784439,1.,0.866025403784439,1.,0.866025403784439,1.,0.866025403784439,
1.,0.866025403784439,1.,0.866025403784439,1.,0.866025403784439,1.,0.866025403784439,
1.,0.866025403784439,1.,0.866025403784439,1.,0.866025403784439,1.,0.866025403784439,
1.,0.866025403784439,1.,0.866025403784439,1.,0.866025403784439,1.,0.866025403784439,
1.,0.866025403784439,1.,0.866025403784439,1.,0.866025403784439,1.,0.866025403784439,
1.,0.866025403784439,1.,0.866025403784439,1.,0.866025403784439,1.,0.866025403784439,
1.,0.866025403784439,1.,0.866025403784439,1.),(0.804737854124365,0.696923425058676,
0.804737854124365,0.696923425058676,0.804737854124365,0.696923425058676,
0.804737854124365,0.696923425058676,0.804737854124365,0.696923425058676,
0.804737854124365,0.696923425058676,0.804737854124365,0.696923425058676,
0.804737854124365,0.696923425058676,0.804737854124365,0.696923425058676,
0.804737854124365,0.696923425058676,0.804737854124365,0.696923425058676,
0.804737854124365,0.696923425058676,0.804737854124365,0.696923425058676,
0.804737854124365,0.696923425058676,0.804737854124365,0.696923425058676,
0.804737854124365,0.696923425058676,0.804737854124365,0.696923425058676,
0.804737854124365,0.696923425058676,0.804737854124365,0.696923425058676,
0.804737854124365,0.696923425058676,0.804737854124365,0.696923425058676,
0.804737854124365,0.696923425058676,0.804737854124365,0.696923425058676,
0.804737854124365,0.696923425058676,0.804737854124365,0.696923425058676,
0.804737854124365,0.696923425058676,0.804737854124365,0.696923425058676,
0.804737854124365,0.696923425058676,0.804737854124365,0.696923425058676,
0.804737854124365,0.696923425058676,0.804737854124365,0.696923425058676,
0.804737854124365,0.696923425058676,0.804737854124365,0.696923425058676,
0.804737854124365,0.696923425058676,0.804737854124365,0.696923425058676,
0.804737854124365,0.696923425058676,0.804737854124365),(0.804737854124365,
0.696923425058676,0.804737854124365,0.696923425058676,0.804737854124365,
0.696923425058676,0.804737854124365,0.696923425058676,0.804737854124365,
0.696923425058676,0.804737854124365,0.696923425058676,0.804737854124365,
0.696923425058676,0.804737854124365,0.696923425058676,0.804737854124365,
0.696923425058676,0.804737854124365,0.696923425058676,0.804737854124365,
0.696923425058676,0.804737854124365,0.696923425058676,0.804737854124365,
0.696923425058676,0.804737854124365,0.696923425058676,0.804737854124365,
0.696923425058676,0.804737854124365,0.696923425058676,0.804737854124365,
0.696923425058676,0.804737854124365,0.696923425058676,0.804737854124365,
0.696923425058676,0.804737854124365,0.696923425058676,0.804737854124365,
0.696923425058676,0.804737854124365,0.696923425058676,0.804737854124365,
0.696923425058676,0.804737854124365,0.696923425058676,0.804737854124365,
0.696923425058676,0.804737854124365,0.696923425058676,0.804737854124365,
0.696923425058676,0.804737854124365,0.696923425058676,0.804737854124365,
0.696923425058676,0.804737854124365,0.696923425058676,0.804737854124365,
0.696923425058676,0.804737854124365,0.696923425058676,0.804737854124365,
0.696923425058676,0.804737854124365,0.696923425058676,0.804737854124365,
0.696923425058676,0.804737854124365,0.696923425058676,0.804737854124365),
(1.,0.866025403784439,1.,0.866025403784439,1.,0.866025403784439,1.,0.866025403784439,
1.,0.866025403784439,1.,0.866025403784439,1.,0.866025403784439,1.,0.866025403784439,
1.,0.866025403784439,1.,0.866025403784439,1.,0.866025403784439,1.,0.866025403784439,
1.,0.866025403784439,1.,0.866025403784439,1.,0.866025403784439,1.,0.866025403784439,
1.,0.866025403784439,1.,0.866025403784439,1.,0.866025403784439,1.,0.866025403784439,
1.,0.866025403784439,1.,0.866025403784439,1.,0.866025403784439,1.,0.866025403784439,
1.,0.866025403784439,1.,0.866025403784439,1.,0.866025403784439,1.,0.866025403784439,
1.,0.866025403784439,1.,0.866025403784439,1.,0.866025403784439,1.,0.866025403784439,
1.,0.866025403784439,1.,0.866025403784439,1.,0.866025403784439,1.,0.866025403784439,
1.)))
REPRESENTATION_ITEM('')
SURFACE()
);
#438=(
BOUNDED_SURFACE()
B_SPLINE_SURFACE(3,2,((#20778,#20779,#20780,#20781,#20782,#20783,#20784,
#20785,#20786,#20787,#20788,#20789,#20790,#20791,#20792,#20793,#20794,#20795,
#20796,#20797,#20798,#20799,#20800,#20801,#20802,#20803,#20804,#20805,#20806,
#20807,#20808,#20809,#20810,#20811,#20812,#20813,#20814,#20815,#20816,#20817,
#20818,#20819,#20820,#20821,#20822,#20823,#20824,#20825,#20826,#20827,#20828,
#20829,#20830,#20831,#20832,#20833,#20834,#20835,#20836,#20837,#20838,#20839,
#20840,#20841,#20842,#20843,#20844,#20845,#20846,#20847,#20848,#20849,#20850),
(#20851,#20852,#20853,#20854,#20855,#20856,#20857,#20858,#20859,#20860,
#20861,#20862,#20863,#20864,#20865,#20866,#20867,#20868,#20869,#20870,#20871,
#20872,#20873,#20874,#20875,#20876,#20877,#20878,#20879,#20880,#20881,#20882,
#20883,#20884,#20885,#20886,#20887,#20888,#20889,#20890,#20891,#20892,#20893,
#20894,#20895,#20896,#20897,#20898,#20899,#20900,#20901,#20902,#20903,#20904,
#20905,#20906,#20907,#20908,#20909,#20910,#20911,#20912,#20913,#20914,#20915,
#20916,#20917,#20918,#20919,#20920,#20921,#20922,#20923),(#20924,#20925,
#20926,#20927,#20928,#20929,#20930,#20931,#20932,#20933,#20934,#20935,#20936,
#20937,#20938,#20939,#20940,#20941,#20942,#20943,#20944,#20945,#20946,#20947,
#20948,#20949,#20950,#20951,#20952,#20953,#20954,#20955,#20956,#20957,#20958,
#20959,#20960,#20961,#20962,#20963,#20964,#20965,#20966,#20967,#20968,#20969,
#20970,#20971,#20972,#20973,#20974,#20975,#20976,#20977,#20978,#20979,#20980,
#20981,#20982,#20983,#20984,#20985,#20986,#20987,#20988,#20989,#20990,#20991,
#20992,#20993,#20994,#20995,#20996),(#20997,#20998,#20999,#21000,#21001,
#21002,#21003,#21004,#21005,#21006,#21007,#21008,#21009,#21010,#21011,#21012,
#21013,#21014,#21015,#21016,#21017,#21018,#21019,#21020,#21021,#21022,#21023,
#21024,#21025,#21026,#21027,#21028,#21029,#21030,#21031,#21032,#21033,#21034,
#21035,#21036,#21037,#21038,#21039,#21040,#21041,#21042,#21043,#21044,#21045,
#21046,#21047,#21048,#21049,#21050,#21051,#21052,#21053,#21054,#21055,#21056,
#21057,#21058,#21059,#21060,#21061,#21062,#21063,#21064,#21065,#21066,#21067,
#21068,#21069)),.UNSPECIFIED.,.F.,.F.,.F.)
B_SPLINE_SURFACE_WITH_KNOTS((4,4),(3,2,2,2,2,2,2,2,2,2,2,2,2,2,2,2,2,2,
2,2,2,2,2,2,2,2,2,2,2,2,2,2,2,2,2,2,3),(0.,1.),(0.,0.0277777777777778,0.0555555555555556,
0.0833333333333333,0.111111111111111,0.138888888888889,0.166666666666667,
0.194444444444444,0.222222222222222,0.25,0.277777777777778,0.305555555555556,
0.333333333333333,0.361111111111111,0.388888888888889,0.416666666666667,
0.444444444444444,0.472222222222222,0.5,0.527777777777778,0.555555555555556,
0.583333333333333,0.611111111111111,0.638888888888889,0.666666666666667,
0.694444444444444,0.722222222222222,0.75,0.777777777777778,0.805555555555556,
0.833333333333333,0.861111111111111,0.888888888888889,0.916666666666667,
0.944444444444444,0.972222222222222,1.),.UNSPECIFIED.)
GEOMETRIC_REPRESENTATION_ITEM()
RATIONAL_B_SPLINE_SURFACE(((1.,0.866025403784439,1.,0.866025403784439,1.,
0.866025403784439,1.,0.866025403784439,1.,0.866025403784439,1.,0.866025403784439,
1.,0.866025403784439,1.,0.866025403784439,1.,0.866025403784439,1.,0.866025403784439,
1.,0.866025403784439,1.,0.866025403784439,1.,0.866025403784439,1.,0.866025403784439,
1.,0.866025403784439,1.,0.866025403784439,1.,0.866025403784439,1.,0.866025403784439,
1.,0.866025403784439,1.,0.866025403784439,1.,0.866025403784439,1.,0.866025403784439,
1.,0.866025403784439,1.,0.866025403784439,1.,0.866025403784439,1.,0.866025403784439,
1.,0.866025403784439,1.,0.866025403784439,1.,0.866025403784439,1.,0.866025403784439,
1.,0.866025403784439,1.,0.866025403784439,1.,0.866025403784439,1.,0.866025403784439,
1.,0.866025403784439,1.,0.866025403784439,1.),(0.804737854124365,0.696923425058676,
0.804737854124365,0.696923425058676,0.804737854124365,0.696923425058676,
0.804737854124365,0.696923425058676,0.804737854124365,0.696923425058676,
0.804737854124365,0.696923425058676,0.804737854124365,0.696923425058676,
0.804737854124365,0.696923425058676,0.804737854124365,0.696923425058676,
0.804737854124365,0.696923425058676,0.804737854124365,0.696923425058676,
0.804737854124365,0.696923425058676,0.804737854124365,0.696923425058676,
0.804737854124365,0.696923425058676,0.804737854124365,0.696923425058676,
0.804737854124365,0.696923425058676,0.804737854124365,0.696923425058676,
0.804737854124365,0.696923425058676,0.804737854124365,0.696923425058676,
0.804737854124365,0.696923425058676,0.804737854124365,0.696923425058676,
0.804737854124365,0.696923425058676,0.804737854124365,0.696923425058676,
0.804737854124365,0.696923425058676,0.804737854124365,0.696923425058676,
0.804737854124365,0.696923425058676,0.804737854124365,0.696923425058676,
0.804737854124365,0.696923425058676,0.804737854124365,0.696923425058676,
0.804737854124365,0.696923425058676,0.804737854124365,0.696923425058676,
0.804737854124365,0.696923425058676,0.804737854124365,0.696923425058676,
0.804737854124365,0.696923425058676,0.804737854124365,0.696923425058676,
0.804737854124365,0.696923425058676,0.804737854124365),(0.804737854124365,
0.696923425058676,0.804737854124365,0.696923425058676,0.804737854124365,
0.696923425058676,0.804737854124365,0.696923425058676,0.804737854124365,
0.696923425058676,0.804737854124365,0.696923425058676,0.804737854124365,
0.696923425058676,0.804737854124365,0.696923425058676,0.804737854124365,
0.696923425058676,0.804737854124365,0.696923425058676,0.804737854124365,
0.696923425058676,0.804737854124365,0.696923425058676,0.804737854124365,
0.696923425058676,0.804737854124365,0.696923425058676,0.804737854124365,
0.696923425058676,0.804737854124365,0.696923425058676,0.804737854124365,
0.696923425058676,0.804737854124365,0.696923425058676,0.804737854124365,
0.696923425058676,0.804737854124365,0.696923425058676,0.804737854124365,
0.696923425058676,0.804737854124365,0.696923425058676,0.804737854124365,
0.696923425058676,0.804737854124365,0.696923425058676,0.804737854124365,
0.696923425058676,0.804737854124365,0.696923425058676,0.804737854124365,
0.696923425058676,0.804737854124365,0.696923425058676,0.804737854124365,
0.696923425058676,0.804737854124365,0.696923425058676,0.804737854124365,
0.696923425058676,0.804737854124365,0.696923425058676,0.804737854124365,
0.696923425058676,0.804737854124365,0.696923425058676,0.804737854124365,
0.696923425058676,0.804737854124365,0.696923425058676,0.804737854124365),
(1.,0.866025403784439,1.,0.866025403784439,1.,0.866025403784439,1.,0.866025403784439,
1.,0.866025403784439,1.,0.866025403784439,1.,0.866025403784439,1.,0.866025403784439,
1.,0.866025403784439,1.,0.866025403784439,1.,0.866025403784439,1.,0.866025403784439,
1.,0.866025403784439,1.,0.866025403784439,1.,0.866025403784439,1.,0.866025403784439,
1.,0.866025403784439,1.,0.866025403784439,1.,0.866025403784439,1.,0.866025403784439,
1.,0.866025403784439,1.,0.866025403784439,1.,0.866025403784439,1.,0.866025403784439,
1.,0.866025403784439,1.,0.866025403784439,1.,0.866025403784439,1.,0.866025403784439,
1.,0.866025403784439,1.,0.866025403784439,1.,0.866025403784439,1.,0.866025403784439,
1.,0.866025403784439,1.,0.866025403784439,1.,0.866025403784439,1.,0.866025403784439,
1.)))
REPRESENTATION_ITEM('')
SURFACE()
);
#439=(
BOUNDED_SURFACE()
B_SPLINE_SURFACE(3,3,((#22265,#22266,#22267,#22268),(#22269,#22270,#22271,
#22272),(#22273,#22274,#22275,#22276),(#22277,#22278,#22279,#22280),(#22281,
#22282,#22283,#22284),(#22285,#22286,#22287,#22288),(#22289,#22290,#22291,
#22292)),.UNSPECIFIED.,.T.,.F.,.F.)
B_SPLINE_SURFACE_WITH_KNOTS((4,3,4),(4,4),(0.,0.5,1.),(-1.90675276406229E-6,
0.0446764713368579),.UNSPECIFIED.)
GEOMETRIC_REPRESENTATION_ITEM()
RATIONAL_B_SPLINE_SURFACE(((1.,1.,1.,1.),(0.333333333333333,0.333333333333333,
0.333333333333333,0.333333333333333),(0.333333333333333,0.333333333333333,
0.333333333333333,0.333333333333333),(1.,1.,1.,1.),(0.333333333333333,0.333333333333333,
0.333333333333333,0.333333333333333),(0.333333333333333,0.333333333333333,
0.333333333333333,0.333333333333333),(1.,1.,1.,1.)))
REPRESENTATION_ITEM('')
SURFACE()
);
#440=(
BOUNDED_SURFACE()
B_SPLINE_SURFACE(3,3,((#22296,#22297,#22298,#22299),(#22300,#22301,#22302,
#22303),(#22304,#22305,#22306,#22307),(#22308,#22309,#22310,#22311),(#22312,
#22313,#22314,#22315),(#22316,#22317,#22318,#22319),(#22320,#22321,#22322,
#22323)),.UNSPECIFIED.,.T.,.F.,.F.)
B_SPLINE_SURFACE_WITH_KNOTS((4,3,4),(4,4),(0.,0.5,1.),(0.955323528663142,
1.00000238460506),.UNSPECIFIED.)
GEOMETRIC_REPRESENTATION_ITEM()
RATIONAL_B_SPLINE_SURFACE(((1.,1.,1.,0.999999999999999),(0.333333333333333,
0.333333333333333,0.333333333333333,0.333333333333333),(0.333333333333333,
0.333333333333333,0.333333333333333,0.333333333333333),(1.,1.,1.,0.999999999999999),
(0.333333333333333,0.333333333333333,0.333333333333333,0.333333333333333),
(0.333333333333333,0.333333333333333,0.333333333333333,0.333333333333333),
(1.,1.,1.,0.999999999999999)))
REPRESENTATION_ITEM('')
SURFACE()
);
#441=(
BOUNDED_SURFACE()
B_SPLINE_SURFACE(3,3,((#22324,#22325,#22326,#22327),(#22328,#22329,#22330,
#22331),(#22332,#22333,#22334,#22335),(#22336,#22337,#22338,#22339),(#22340,
#22341,#22342,#22343),(#22344,#22345,#22346,#22347),(#22348,#22349,#22350,
#22351)),.UNSPECIFIED.,.T.,.F.,.F.)
B_SPLINE_SURFACE_WITH_KNOTS((4,3,4),(4,4),(0.,0.5,1.),(-1.90675276411689E-6,
0.044676471336858),.UNSPECIFIED.)
GEOMETRIC_REPRESENTATION_ITEM()
RATIONAL_B_SPLINE_SURFACE(((0.999999999999999,1.,1.,1.),(0.333333333333333,
0.333333333333333,0.333333333333333,0.333333333333333),(0.333333333333333,
0.333333333333333,0.333333333333333,0.333333333333333),(0.999999999999999,
1.,1.,1.),(0.333333333333333,0.333333333333333,0.333333333333333,0.333333333333333),
(0.333333333333333,0.333333333333333,0.333333333333333,0.333333333333333),
(0.999999999999999,1.,1.,1.)))
REPRESENTATION_ITEM('')
SURFACE()
);
#442=(
BOUNDED_SURFACE()
B_SPLINE_SURFACE(3,3,((#22355,#22356,#22357,#22358),(#22359,#22360,#22361,
#22362),(#22363,#22364,#22365,#22366),(#22367,#22368,#22369,#22370),(#22371,
#22372,#22373,#22374),(#22375,#22376,#22377,#22378),(#22379,#22380,#22381,
#22382)),.UNSPECIFIED.,.T.,.F.,.F.)
B_SPLINE_SURFACE_WITH_KNOTS((4,3,4),(4,4),(0.,0.5,1.),(0.955323528663142,
1.00000238460506),.UNSPECIFIED.)
GEOMETRIC_REPRESENTATION_ITEM()
RATIONAL_B_SPLINE_SURFACE(((1.,1.,1.,1.),(0.333333333333333,0.333333333333333,
0.333333333333333,0.333333333333333),(0.333333333333333,0.333333333333333,
0.333333333333333,0.333333333333333),(1.,1.,1.,1.),(0.333333333333333,0.333333333333333,
0.333333333333333,0.333333333333333),(0.333333333333333,0.333333333333333,
0.333333333333333,0.333333333333333),(1.,1.,1.,1.)))
REPRESENTATION_ITEM('')
SURFACE()
);
#443=(
BOUNDED_SURFACE()
B_SPLINE_SURFACE(3,3,((#22383,#22384,#22385,#22386),(#22387,#22388,#22389,
#22390),(#22391,#22392,#22393,#22394),(#22395,#22396,#22397,#22398),(#22399,
#22400,#22401,#22402),(#22403,#22404,#22405,#22406),(#22407,#22408,#22409,
#22410)),.UNSPECIFIED.,.T.,.F.,.F.)
B_SPLINE_SURFACE_WITH_KNOTS((4,3,4),(4,4),(0.,0.5,1.),(-1.90675276402769E-6,
0.044676471336858),.UNSPECIFIED.)
GEOMETRIC_REPRESENTATION_ITEM()
RATIONAL_B_SPLINE_SURFACE(((1.,1.,1.,1.),(0.333333333333334,0.333333333333333,
0.333333333333333,0.333333333333333),(0.333333333333334,0.333333333333333,
0.333333333333333,0.333333333333333),(1.,1.,1.,1.),(0.333333333333334,0.333333333333333,
0.333333333333333,0.333333333333333),(0.333333333333334,0.333333333333333,
0.333333333333333,0.333333333333333),(1.,1.,1.,1.)))
REPRESENTATION_ITEM('')
SURFACE()
);
#444=(
BOUNDED_SURFACE()
B_SPLINE_SURFACE(3,3,((#22414,#22415,#22416,#22417),(#22418,#22419,#22420,
#22421),(#22422,#22423,#22424,#22425),(#22426,#22427,#22428,#22429),(#22430,
#22431,#22432,#22433),(#22434,#22435,#22436,#22437),(#22438,#22439,#22440,
#22441)),.UNSPECIFIED.,.T.,.F.,.F.)
B_SPLINE_SURFACE_WITH_KNOTS((4,3,4),(4,4),(0.,0.5,1.),(0.955323528663142,
1.00000238460506),.UNSPECIFIED.)
GEOMETRIC_REPRESENTATION_ITEM()
RATIONAL_B_SPLINE_SURFACE(((1.,1.,1.,1.),(0.333333333333333,0.333333333333333,
0.333333333333333,0.333333333333333),(0.333333333333333,0.333333333333333,
0.333333333333333,0.333333333333333),(1.,1.,1.,1.),(0.333333333333333,0.333333333333333,
0.333333333333333,0.333333333333333),(0.333333333333333,0.333333333333333,
0.333333333333333,0.333333333333333),(1.,1.,1.,1.)))
REPRESENTATION_ITEM('')
SURFACE()
);
#445=(
BOUNDED_SURFACE()
B_SPLINE_SURFACE(3,3,((#22442,#22443,#22444,#22445),(#22446,#22447,#22448,
#22449),(#22450,#22451,#22452,#22453),(#22454,#22455,#22456,#22457),(#22458,
#22459,#22460,#22461),(#22462,#22463,#22464,#22465),(#22466,#22467,#22468,
#22469)),.UNSPECIFIED.,.T.,.F.,.F.)
B_SPLINE_SURFACE_WITH_KNOTS((4,3,4),(4,4),(0.,0.5,1.),(-1.90675276440842E-6,
0.0446764713368579),.UNSPECIFIED.)
GEOMETRIC_REPRESENTATION_ITEM()
RATIONAL_B_SPLINE_SURFACE(((1.,1.,1.,1.),(0.333333333333333,0.333333333333333,
0.333333333333333,0.333333333333333),(0.333333333333333,0.333333333333333,
0.333333333333333,0.333333333333333),(1.,1.,1.,1.),(0.333333333333333,0.333333333333333,
0.333333333333333,0.333333333333333),(0.333333333333333,0.333333333333333,
0.333333333333333,0.333333333333333),(1.,1.,1.,1.)))
REPRESENTATION_ITEM('')
SURFACE()
);
#446=(
BOUNDED_SURFACE()
B_SPLINE_SURFACE(3,3,((#22473,#22474,#22475,#22476),(#22477,#22478,#22479,
#22480),(#22481,#22482,#22483,#22484),(#22485,#22486,#22487,#22488),(#22489,
#22490,#22491,#22492),(#22493,#22494,#22495,#22496),(#22497,#22498,#22499,
#22500)),.UNSPECIFIED.,.T.,.F.,.F.)
B_SPLINE_SURFACE_WITH_KNOTS((4,3,4),(4,4),(0.,0.5,1.),(0.955323528663142,
1.00000238460506),.UNSPECIFIED.)
GEOMETRIC_REPRESENTATION_ITEM()
RATIONAL_B_SPLINE_SURFACE(((1.,1.,1.,1.),(0.333333333333333,0.333333333333333,
0.333333333333333,0.333333333333333),(0.333333333333333,0.333333333333333,
0.333333333333333,0.333333333333333),(1.,1.,1.,1.),(0.333333333333333,0.333333333333333,
0.333333333333333,0.333333333333333),(0.333333333333333,0.333333333333333,
0.333333333333333,0.333333333333333),(1.,1.,1.,1.)))
REPRESENTATION_ITEM('')
SURFACE()
);
#447=(
BOUNDED_SURFACE()
B_SPLINE_SURFACE(3,3,((#22501,#22502,#22503,#22504),(#22505,#22506,#22507,
#22508),(#22509,#22510,#22511,#22512),(#22513,#22514,#22515,#22516),(#22517,
#22518,#22519,#22520),(#22521,#22522,#22523,#22524),(#22525,#22526,#22527,
#22528)),.UNSPECIFIED.,.T.,.F.,.F.)
B_SPLINE_SURFACE_WITH_KNOTS((4,3,4),(4,4),(0.,0.5,1.),(-1.90675276415042E-6,
0.0446764713368579),.UNSPECIFIED.)
GEOMETRIC_REPRESENTATION_ITEM()
RATIONAL_B_SPLINE_SURFACE(((1.,1.,1.,1.),(0.333333333333333,0.333333333333333,
0.333333333333333,0.333333333333333),(0.333333333333333,0.333333333333333,
0.333333333333333,0.333333333333333),(1.,1.,1.,1.),(0.333333333333333,0.333333333333333,
0.333333333333333,0.333333333333333),(0.333333333333333,0.333333333333333,
0.333333333333333,0.333333333333333),(1.,1.,1.,1.)))
REPRESENTATION_ITEM('')
SURFACE()
);
#448=(
BOUNDED_SURFACE()
B_SPLINE_SURFACE(3,3,((#22532,#22533,#22534,#22535),(#22536,#22537,#22538,
#22539),(#22540,#22541,#22542,#22543),(#22544,#22545,#22546,#22547),(#22548,
#22549,#22550,#22551),(#22552,#22553,#22554,#22555),(#22556,#22557,#22558,
#22559)),.UNSPECIFIED.,.T.,.F.,.F.)
B_SPLINE_SURFACE_WITH_KNOTS((4,3,4),(4,4),(0.,0.5,1.),(0.955323528663142,
1.00000238460506),.UNSPECIFIED.)
GEOMETRIC_REPRESENTATION_ITEM()
RATIONAL_B_SPLINE_SURFACE(((1.,1.,1.,1.),(0.333333333333333,0.333333333333333,
0.333333333333333,0.333333333333333),(0.333333333333333,0.333333333333333,
0.333333333333333,0.333333333333333),(1.,1.,1.,1.),(0.333333333333333,0.333333333333333,
0.333333333333333,0.333333333333333),(0.333333333333333,0.333333333333333,
0.333333333333333,0.333333333333333),(1.,1.,1.,1.)))
REPRESENTATION_ITEM('')
SURFACE()
);
#449=(
BOUNDED_SURFACE()
B_SPLINE_SURFACE(3,3,((#22560,#22561,#22562,#22563),(#22564,#22565,#22566,
#22567),(#22568,#22569,#22570,#22571),(#22572,#22573,#22574,#22575),(#22576,
#22577,#22578,#22579),(#22580,#22581,#22582,#22583),(#22584,#22585,#22586,
#22587)),.UNSPECIFIED.,.T.,.F.,.F.)
B_SPLINE_SURFACE_WITH_KNOTS((4,3,4),(4,4),(0.,0.5,1.),(-1.90675276405256E-6,
0.0446764713368579),.UNSPECIFIED.)
GEOMETRIC_REPRESENTATION_ITEM()
RATIONAL_B_SPLINE_SURFACE(((1.,1.,1.,1.),(0.333333333333333,0.333333333333333,
0.333333333333333,0.333333333333333),(0.333333333333333,0.333333333333333,
0.333333333333333,0.333333333333333),(1.,1.,1.,1.),(0.333333333333333,0.333333333333333,
0.333333333333333,0.333333333333333),(0.333333333333333,0.333333333333333,
0.333333333333333,0.333333333333333),(1.,1.,1.,1.)))
REPRESENTATION_ITEM('')
SURFACE()
);
#450=(
BOUNDED_SURFACE()
B_SPLINE_SURFACE(3,3,((#22591,#22592,#22593,#22594),(#22595,#22596,#22597,
#22598),(#22599,#22600,#22601,#22602),(#22603,#22604,#22605,#22606),(#22607,
#22608,#22609,#22610),(#22611,#22612,#22613,#22614),(#22615,#22616,#22617,
#22618)),.UNSPECIFIED.,.T.,.F.,.F.)
B_SPLINE_SURFACE_WITH_KNOTS((4,3,4),(4,4),(0.,0.5,1.),(0.955323528663142,
1.00000238460506),.UNSPECIFIED.)
GEOMETRIC_REPRESENTATION_ITEM()
RATIONAL_B_SPLINE_SURFACE(((1.,1.,1.,0.999999999999999),(0.333333333333333,
0.333333333333333,0.333333333333333,0.333333333333333),(0.333333333333333,
0.333333333333333,0.333333333333333,0.333333333333333),(1.,1.,1.,0.999999999999999),
(0.333333333333333,0.333333333333333,0.333333333333333,0.333333333333333),
(0.333333333333333,0.333333333333333,0.333333333333333,0.333333333333333),
(1.,1.,1.,0.999999999999999)))
REPRESENTATION_ITEM('')
SURFACE()
);
#451=(
BOUNDED_SURFACE()
B_SPLINE_SURFACE(3,3,((#22619,#22620,#22621,#22622),(#22623,#22624,#22625,
#22626),(#22627,#22628,#22629,#22630),(#22631,#22632,#22633,#22634),(#22635,
#22636,#22637,#22638),(#22639,#22640,#22641,#22642),(#22643,#22644,#22645,
#22646)),.UNSPECIFIED.,.T.,.F.,.F.)
B_SPLINE_SURFACE_WITH_KNOTS((4,3,4),(4,4),(0.,0.5,1.),(-1.90675276426259E-6,
0.0446764713368579),.UNSPECIFIED.)
GEOMETRIC_REPRESENTATION_ITEM()
RATIONAL_B_SPLINE_SURFACE(((1.,1.,1.,1.),(0.333333333333333,0.333333333333333,
0.333333333333333,0.333333333333333),(0.333333333333333,0.333333333333333,
0.333333333333333,0.333333333333333),(1.,1.,1.,1.),(0.333333333333333,0.333333333333333,
0.333333333333333,0.333333333333333),(0.333333333333333,0.333333333333333,
0.333333333333333,0.333333333333333),(1.,1.,1.,1.)))
REPRESENTATION_ITEM('')
SURFACE()
);
#452=(
BOUNDED_SURFACE()
B_SPLINE_SURFACE(3,3,((#22650,#22651,#22652,#22653),(#22654,#22655,#22656,
#22657),(#22658,#22659,#22660,#22661),(#22662,#22663,#22664,#22665),(#22666,
#22667,#22668,#22669),(#22670,#22671,#22672,#22673),(#22674,#22675,#22676,
#22677)),.UNSPECIFIED.,.T.,.F.,.F.)
B_SPLINE_SURFACE_WITH_KNOTS((4,3,4),(4,4),(0.,0.5,1.),(0.955323528663142,
1.00000238460506),.UNSPECIFIED.)
GEOMETRIC_REPRESENTATION_ITEM()
RATIONAL_B_SPLINE_SURFACE(((1.,1.,1.,1.),(0.333333333333333,0.333333333333333,
0.333333333333333,0.333333333333333),(0.333333333333333,0.333333333333333,
0.333333333333333,0.333333333333333),(1.,1.,1.,1.),(0.333333333333333,0.333333333333333,
0.333333333333333,0.333333333333333),(0.333333333333333,0.333333333333333,
0.333333333333333,0.333333333333333),(1.,1.,1.,1.)))
REPRESENTATION_ITEM('')
SURFACE()
);
#453=(
BOUNDED_SURFACE()
B_SPLINE_SURFACE(3,3,((#22678,#22679,#22680,#22681),(#22682,#22683,#22684,
#22685),(#22686,#22687,#22688,#22689),(#22690,#22691,#22692,#22693),(#22694,
#22695,#22696,#22697),(#22698,#22699,#22700,#22701),(#22702,#22703,#22704,
#22705)),.UNSPECIFIED.,.T.,.F.,.F.)
B_SPLINE_SURFACE_WITH_KNOTS((4,3,4),(4,4),(0.,0.5,1.),(-1.90675276424112E-6,
0.0446764713368579),.UNSPECIFIED.)
GEOMETRIC_REPRESENTATION_ITEM()
RATIONAL_B_SPLINE_SURFACE(((1.,1.,1.,1.),(0.333333333333333,0.333333333333333,
0.333333333333333,0.333333333333333),(0.333333333333333,0.333333333333333,
0.333333333333333,0.333333333333333),(1.,1.,1.,1.),(0.333333333333333,0.333333333333333,
0.333333333333333,0.333333333333333),(0.333333333333333,0.333333333333333,
0.333333333333333,0.333333333333333),(1.,1.,1.,1.)))
REPRESENTATION_ITEM('')
SURFACE()
);
#454=(
BOUNDED_SURFACE()
B_SPLINE_SURFACE(3,3,((#22709,#22710,#22711,#22712),(#22713,#22714,#22715,
#22716),(#22717,#22718,#22719,#22720),(#22721,#22722,#22723,#22724),(#22725,
#22726,#22727,#22728),(#22729,#22730,#22731,#22732),(#22733,#22734,#22735,
#22736)),.UNSPECIFIED.,.T.,.F.,.F.)
B_SPLINE_SURFACE_WITH_KNOTS((4,3,4),(4,4),(0.,0.5,1.),(0.955323528663142,
1.00000238460506),.UNSPECIFIED.)
GEOMETRIC_REPRESENTATION_ITEM()
RATIONAL_B_SPLINE_SURFACE(((1.,1.,1.,0.999999999999999),(0.333333333333333,
0.333333333333333,0.333333333333333,0.333333333333333),(0.333333333333333,
0.333333333333333,0.333333333333333,0.333333333333333),(1.,1.,1.,0.999999999999999),
(0.333333333333333,0.333333333333333,0.333333333333333,0.333333333333333),
(0.333333333333333,0.333333333333333,0.333333333333333,0.333333333333333),
(1.,1.,1.,0.999999999999999)))
REPRESENTATION_ITEM('')
SURFACE()
);
#455=(
BOUNDED_SURFACE()
B_SPLINE_SURFACE(3,3,((#22737,#22738,#22739,#22740),(#22741,#22742,#22743,
#22744),(#22745,#22746,#22747,#22748),(#22749,#22750,#22751,#22752),(#22753,
#22754,#22755,#22756),(#22757,#22758,#22759,#22760),(#22761,#22762,#22763,
#22764)),.UNSPECIFIED.,.T.,.F.,.F.)
B_SPLINE_SURFACE_WITH_KNOTS((4,3,4),(4,4),(0.,0.5,1.),(-1.90675276443097E-6,
0.0446764713368579),.UNSPECIFIED.)
GEOMETRIC_REPRESENTATION_ITEM()
RATIONAL_B_SPLINE_SURFACE(((1.,1.,1.,1.),(0.333333333333333,0.333333333333333,
0.333333333333333,0.333333333333333),(0.333333333333333,0.333333333333333,
0.333333333333333,0.333333333333333),(1.,1.,1.,1.),(0.333333333333333,0.333333333333333,
0.333333333333333,0.333333333333333),(0.333333333333333,0.333333333333333,
0.333333333333333,0.333333333333333),(1.,1.,1.,1.)))
REPRESENTATION_ITEM('')
SURFACE()
);
#456=(
BOUNDED_SURFACE()
B_SPLINE_SURFACE(3,3,((#22768,#22769,#22770,#22771),(#22772,#22773,#22774,
#22775),(#22776,#22777,#22778,#22779),(#22780,#22781,#22782,#22783),(#22784,
#22785,#22786,#22787),(#22788,#22789,#22790,#22791),(#22792,#22793,#22794,
#22795)),.UNSPECIFIED.,.T.,.F.,.F.)
B_SPLINE_SURFACE_WITH_KNOTS((4,3,4),(4,4),(0.,0.5,1.),(0.955323528663142,
1.00000238460506),.UNSPECIFIED.)
GEOMETRIC_REPRESENTATION_ITEM()
RATIONAL_B_SPLINE_SURFACE(((1.,1.,1.,1.),(0.333333333333333,0.333333333333333,
0.333333333333333,0.333333333333333),(0.333333333333333,0.333333333333333,
0.333333333333333,0.333333333333333),(1.,1.,1.,1.),(0.333333333333333,0.333333333333333,
0.333333333333333,0.333333333333333),(0.333333333333333,0.333333333333333,
0.333333333333333,0.333333333333333),(1.,1.,1.,1.)))
REPRESENTATION_ITEM('')
SURFACE()
);
#457=(
BOUNDED_SURFACE()
B_SPLINE_SURFACE(3,3,((#22796,#22797,#22798,#22799),(#22800,#22801,#22802,
#22803),(#22804,#22805,#22806,#22807),(#22808,#22809,#22810,#22811),(#22812,
#22813,#22814,#22815),(#22816,#22817,#22818,#22819),(#22820,#22821,#22822,
#22823)),.UNSPECIFIED.,.T.,.F.,.F.)
B_SPLINE_SURFACE_WITH_KNOTS((4,3,4),(4,4),(0.,0.5,1.),(-1.90675276401703E-6,
0.0446764713368579),.UNSPECIFIED.)
GEOMETRIC_REPRESENTATION_ITEM()
RATIONAL_B_SPLINE_SURFACE(((0.999999999999999,1.,1.,1.),(0.333333333333333,
0.333333333333333,0.333333333333333,0.333333333333333),(0.333333333333333,
0.333333333333333,0.333333333333333,0.333333333333333),(0.999999999999999,
1.,1.,1.),(0.333333333333333,0.333333333333333,0.333333333333333,0.333333333333333),
(0.333333333333333,0.333333333333333,0.333333333333333,0.333333333333333),
(0.999999999999999,1.,1.,1.)))
REPRESENTATION_ITEM('')
SURFACE()
);
#458=(
BOUNDED_SURFACE()
B_SPLINE_SURFACE(3,3,((#22827,#22828,#22829,#22830),(#22831,#22832,#22833,
#22834),(#22835,#22836,#22837,#22838),(#22839,#22840,#22841,#22842),(#22843,
#22844,#22845,#22846),(#22847,#22848,#22849,#22850),(#22851,#22852,#22853,
#22854)),.UNSPECIFIED.,.T.,.F.,.F.)
B_SPLINE_SURFACE_WITH_KNOTS((4,3,4),(4,4),(0.,0.5,1.),(0.955323528663142,
1.00000238460506),.UNSPECIFIED.)
GEOMETRIC_REPRESENTATION_ITEM()
RATIONAL_B_SPLINE_SURFACE(((1.,1.,1.,1.),(0.333333333333333,0.333333333333333,
0.333333333333333,0.333333333333333),(0.333333333333333,0.333333333333333,
0.333333333333333,0.333333333333333),(1.,1.,1.,1.),(0.333333333333333,0.333333333333333,
0.333333333333333,0.333333333333333),(0.333333333333333,0.333333333333333,
0.333333333333333,0.333333333333333),(1.,1.,1.,1.)))
REPRESENTATION_ITEM('')
SURFACE()
);
#459=(
BOUNDED_SURFACE()
B_SPLINE_SURFACE(3,2,((#23960,#23961,#23962,#23963,#23964,#23965,#23966,
#23967,#23968,#23969,#23970,#23971,#23972,#23973,#23974,#23975,#23976,#23977,
#23978,#23979,#23980,#23981,#23982,#23983,#23984,#23985,#23986,#23987,#23988,
#23989,#23990,#23991,#23992,#23993,#23994,#23995,#23996,#23997,#23998,#23999,
#24000,#24001,#24002,#24003,#24004,#24005,#24006,#24007,#24008,#24009,#24010,
#24011,#24012,#24013,#24014,#24015,#24016,#24017,#24018,#24019,#24020,#24021,
#24022,#24023,#24024,#24025,#24026,#24027,#24028,#24029,#24030,#24031,#24032,
#24033,#24034,#24035,#24036,#24037,#24038,#24039,#24040,#24041,#24042,#24043,
#24044,#24045,#24046,#24047,#24048,#24049,#24050,#24051,#24052,#24053,#24054,
#24055,#24056,#24057,#24058,#24059,#24060,#24061,#24062,#24063,#24064,#24065,
#24066,#24067,#24068,#24069,#24070,#24071,#24072,#24073,#24074,#24075,#24076,
#24077,#24078,#24079,#24080,#24081,#24082,#24083,#24084,#24085,#24086,#24087,
#24088,#24089,#24090,#24091,#24092,#24093,#24094,#24095,#24096,#24097,#24098,
#24099,#24100,#24101,#24102,#24103,#24104,#24105,#24106,#24107,#24108,#24109,
#24110,#24111,#24112,#24113,#24114,#24115,#24116,#24117,#24118,#24119,#24120,
#24121,#24122,#24123,#24124,#24125,#24126,#24127,#24128,#24129,#24130,#24131,
#24132,#24133,#24134,#24135,#24136,#24137,#24138,#24139,#24140,#24141,#24142,
#24143,#24144,#24145,#24146,#24147,#24148,#24149,#24150,#24151,#24152,#24153,
#24154,#24155,#24156,#24157,#24158,#24159,#24160,#24161,#24162,#24163,#24164,
#24165,#24166,#24167,#24168,#24169,#24170,#24171,#24172,#24173,#24174,#24175,
#24176,#24177,#24178,#24179,#24180,#24181,#24182,#24183,#24184,#24185,#24186,
#24187,#24188,#24189,#24190,#24191,#24192,#24193,#24194,#24195,#24196,#24197,
#24198,#24199,#24200,#24201,#24202,#24203,#24204,#24205,#24206,#24207,#24208,
#24209,#24210,#24211,#24212,#24213,#24214,#24215,#24216,#24217,#24218,#24219,
#24220,#24221,#24222,#24223,#24224,#24225,#24226,#24227,#24228,#24229,#24230,
#24231,#24232,#24233,#24234,#24235,#24236,#24237,#24238,#24239,#24240,#24241,
#24242,#24243,#24244,#24245,#24246,#24247,#24248,#24249,#24250,#24251,#24252,
#24253,#24254,#24255,#24256,#24257,#24258,#24259,#24260,#24261,#24262,#24263,
#24264,#24265,#24266,#24267,#24268,#24269,#24270,#24271,#24272,#24273,#24274,
#24275,#24276,#24277,#24278,#24279,#24280,#24281,#24282,#24283,#24284,#24285,
#24286,#24287,#24288,#24289,#24290,#24291,#24292,#24293,#24294,#24295,#24296,
#24297,#24298,#24299,#24300,#24301,#24302,#24303,#24304,#24305,#24306,#24307,
#24308,#24309,#24310,#24311,#24312,#24313,#24314,#24315,#24316,#24317,#24318,
#24319,#24320,#24321,#24322,#24323,#24324,#24325,#24326,#24327,#24328,#24329,
#24330,#24331,#24332,#24333,#24334,#24335,#24336,#24337,#24338,#24339,#24340,
#24341,#24342,#24343,#24344,#24345,#24346,#24347,#24348,#24349,#24350,#24351,
#24352,#24353,#24354,#24355,#24356,#24357,#24358,#24359,#24360,#24361,#24362,
#24363,#24364,#24365,#24366,#24367,#24368,#24369,#24370,#24371,#24372,#24373,
#24374,#24375,#24376,#24377,#24378,#24379,#24380,#24381,#24382,#24383,#24384,
#24385,#24386,#24387,#24388,#24389,#24390,#24391,#24392,#24393,#24394,#24395,
#24396,#24397,#24398,#24399,#24400,#24401,#24402,#24403,#24404,#24405,#24406,
#24407,#24408,#24409,#24410,#24411,#24412,#24413,#24414,#24415,#24416),
(#24417,#24418,#24419,#24420,#24421,#24422,#24423,#24424,#24425,#24426,
#24427,#24428,#24429,#24430,#24431,#24432,#24433,#24434,#24435,#24436,#24437,
#24438,#24439,#24440,#24441,#24442,#24443,#24444,#24445,#24446,#24447,#24448,
#24449,#24450,#24451,#24452,#24453,#24454,#24455,#24456,#24457,#24458,#24459,
#24460,#24461,#24462,#24463,#24464,#24465,#24466,#24467,#24468,#24469,#24470,
#24471,#24472,#24473,#24474,#24475,#24476,#24477,#24478,#24479,#24480,#24481,
#24482,#24483,#24484,#24485,#24486,#24487,#24488,#24489,#24490,#24491,#24492,
#24493,#24494,#24495,#24496,#24497,#24498,#24499,#24500,#24501,#24502,#24503,
#24504,#24505,#24506,#24507,#24508,#24509,#24510,#24511,#24512,#24513,#24514,
#24515,#24516,#24517,#24518,#24519,#24520,#24521,#24522,#24523,#24524,#24525,
#24526,#24527,#24528,#24529,#24530,#24531,#24532,#24533,#24534,#24535,#24536,
#24537,#24538,#24539,#24540,#24541,#24542,#24543,#24544,#24545,#24546,#24547,
#24548,#24549,#24550,#24551,#24552,#24553,#24554,#24555,#24556,#24557,#24558,
#24559,#24560,#24561,#24562,#24563,#24564,#24565,#24566,#24567,#24568,#24569,
#24570,#24571,#24572,#24573,#24574,#24575,#24576,#24577,#24578,#24579,#24580,
#24581,#24582,#24583,#24584,#24585,#24586,#24587,#24588,#24589,#24590,#24591,
#24592,#24593,#24594,#24595,#24596,#24597,#24598,#24599,#24600,#24601,#24602,
#24603,#24604,#24605,#24606,#24607,#24608,#24609,#24610,#24611,#24612,#24613,
#24614,#24615,#24616,#24617,#24618,#24619,#24620,#24621,#24622,#24623,#24624,
#24625,#24626,#24627,#24628,#24629,#24630,#24631,#24632,#24633,#24634,#24635,
#24636,#24637,#24638,#24639,#24640,#24641,#24642,#24643,#24644,#24645,#24646,
#24647,#24648,#24649,#24650,#24651,#24652,#24653,#24654,#24655,#24656,#24657,
#24658,#24659,#24660,#24661,#24662,#24663,#24664,#24665,#24666,#24667,#24668,
#24669,#24670,#24671,#24672,#24673,#24674,#24675,#24676,#24677,#24678,#24679,
#24680,#24681,#24682,#24683,#24684,#24685,#24686,#24687,#24688,#24689,#24690,
#24691,#24692,#24693,#24694,#24695,#24696,#24697,#24698,#24699,#24700,#24701,
#24702,#24703,#24704,#24705,#24706,#24707,#24708,#24709,#24710,#24711,#24712,
#24713,#24714,#24715,#24716,#24717,#24718,#24719,#24720,#24721,#24722,#24723,
#24724,#24725,#24726,#24727,#24728,#24729,#24730,#24731,#24732,#24733,#24734,
#24735,#24736,#24737,#24738,#24739,#24740,#24741,#24742,#24743,#24744,#24745,
#24746,#24747,#24748,#24749,#24750,#24751,#24752,#24753,#24754,#24755,#24756,
#24757,#24758,#24759,#24760,#24761,#24762,#24763,#24764,#24765,#24766,#24767,
#24768,#24769,#24770,#24771,#24772,#24773,#24774,#24775,#24776,#24777,#24778,
#24779,#24780,#24781,#24782,#24783,#24784,#24785,#24786,#24787,#24788,#24789,
#24790,#24791,#24792,#24793,#24794,#24795,#24796,#24797,#24798,#24799,#24800,
#24801,#24802,#24803,#24804,#24805,#24806,#24807,#24808,#24809,#24810,#24811,
#24812,#24813,#24814,#24815,#24816,#24817,#24818,#24819,#24820,#24821,#24822,
#24823,#24824,#24825,#24826,#24827,#24828,#24829,#24830,#24831,#24832,#24833,
#24834,#24835,#24836,#24837,#24838,#24839,#24840,#24841,#24842,#24843,#24844,
#24845,#24846,#24847,#24848,#24849,#24850,#24851,#24852,#24853,#24854,#24855,
#24856,#24857,#24858,#24859,#24860,#24861,#24862,#24863,#24864,#24865,#24866,
#24867,#24868,#24869,#24870,#24871,#24872,#24873),(#24874,#24875,#24876,
#24877,#24878,#24879,#24880,#24881,#24882,#24883,#24884,#24885,#24886,#24887,
#24888,#24889,#24890,#24891,#24892,#24893,#24894,#24895,#24896,#24897,#24898,
#24899,#24900,#24901,#24902,#24903,#24904,#24905,#24906,#24907,#24908,#24909,
#24910,#24911,#24912,#24913,#24914,#24915,#24916,#24917,#24918,#24919,#24920,
#24921,#24922,#24923,#24924,#24925,#24926,#24927,#24928,#24929,#24930,#24931,
#24932,#24933,#24934,#24935,#24936,#24937,#24938,#24939,#24940,#24941,#24942,
#24943,#24944,#24945,#24946,#24947,#24948,#24949,#24950,#24951,#24952,#24953,
#24954,#24955,#24956,#24957,#24958,#24959,#24960,#24961,#24962,#24963,#24964,
#24965,#24966,#24967,#24968,#24969,#24970,#24971,#24972,#24973,#24974,#24975,
#24976,#24977,#24978,#24979,#24980,#24981,#24982,#24983,#24984,#24985,#24986,
#24987,#24988,#24989,#24990,#24991,#24992,#24993,#24994,#24995,#24996,#24997,
#24998,#24999,#25000,#25001,#25002,#25003,#25004,#25005,#25006,#25007,#25008,
#25009,#25010,#25011,#25012,#25013,#25014,#25015,#25016,#25017,#25018,#25019,
#25020,#25021,#25022,#25023,#25024,#25025,#25026,#25027,#25028,#25029,#25030,
#25031,#25032,#25033,#25034,#25035,#25036,#25037,#25038,#25039,#25040,#25041,
#25042,#25043,#25044,#25045,#25046,#25047,#25048,#25049,#25050,#25051,#25052,
#25053,#25054,#25055,#25056,#25057,#25058,#25059,#25060,#25061,#25062,#25063,
#25064,#25065,#25066,#25067,#25068,#25069,#25070,#25071,#25072,#25073,#25074,
#25075,#25076,#25077,#25078,#25079,#25080,#25081,#25082,#25083,#25084,#25085,
#25086,#25087,#25088,#25089,#25090,#25091,#25092,#25093,#25094,#25095,#25096,
#25097,#25098,#25099,#25100,#25101,#25102,#25103,#25104,#25105,#25106,#25107,
#25108,#25109,#25110,#25111,#25112,#25113,#25114,#25115,#25116,#25117,#25118,
#25119,#25120,#25121,#25122,#25123,#25124,#25125,#25126,#25127,#25128,#25129,
#25130,#25131,#25132,#25133,#25134,#25135,#25136,#25137,#25138,#25139,#25140,
#25141,#25142,#25143,#25144,#25145,#25146,#25147,#25148,#25149,#25150,#25151,
#25152,#25153,#25154,#25155,#25156,#25157,#25158,#25159,#25160,#25161,#25162,
#25163,#25164,#25165,#25166,#25167,#25168,#25169,#25170,#25171,#25172,#25173,
#25174,#25175,#25176,#25177,#25178,#25179,#25180,#25181,#25182,#25183,#25184,
#25185,#25186,#25187,#25188,#25189,#25190,#25191,#25192,#25193,#25194,#25195,
#25196,#25197,#25198,#25199,#25200,#25201,#25202,#25203,#25204,#25205,#25206,
#25207,#25208,#25209,#25210,#25211,#25212,#25213,#25214,#25215,#25216,#25217,
#25218,#25219,#25220,#25221,#25222,#25223,#25224,#25225,#25226,#25227,#25228,
#25229,#25230,#25231,#25232,#25233,#25234,#25235,#25236,#25237,#25238,#25239,
#25240,#25241,#25242,#25243,#25244,#25245,#25246,#25247,#25248,#25249,#25250,
#25251,#25252,#25253,#25254,#25255,#25256,#25257,#25258,#25259,#25260,#25261,
#25262,#25263,#25264,#25265,#25266,#25267,#25268,#25269,#25270,#25271,#25272,
#25273,#25274,#25275,#25276,#25277,#25278,#25279,#25280,#25281,#25282,#25283,
#25284,#25285,#25286,#25287,#25288,#25289,#25290,#25291,#25292,#25293,#25294,
#25295,#25296,#25297,#25298,#25299,#25300,#25301,#25302,#25303,#25304,#25305,
#25306,#25307,#25308,#25309,#25310,#25311,#25312,#25313,#25314,#25315,#25316,
#25317,#25318,#25319,#25320,#25321,#25322,#25323,#25324,#25325,#25326,#25327,
#25328,#25329,#25330),(#25331,#25332,#25333,#25334,#25335,#25336,#25337,
#25338,#25339,#25340,#25341,#25342,#25343,#25344,#25345,#25346,#25347,#25348,
#25349,#25350,#25351,#25352,#25353,#25354,#25355,#25356,#25357,#25358,#25359,
#25360,#25361,#25362,#25363,#25364,#25365,#25366,#25367,#25368,#25369,#25370,
#25371,#25372,#25373,#25374,#25375,#25376,#25377,#25378,#25379,#25380,#25381,
#25382,#25383,#25384,#25385,#25386,#25387,#25388,#25389,#25390,#25391,#25392,
#25393,#25394,#25395,#25396,#25397,#25398,#25399,#25400,#25401,#25402,#25403,
#25404,#25405,#25406,#25407,#25408,#25409,#25410,#25411,#25412,#25413,#25414,
#25415,#25416,#25417,#25418,#25419,#25420,#25421,#25422,#25423,#25424,#25425,
#25426,#25427,#25428,#25429,#25430,#25431,#25432,#25433,#25434,#25435,#25436,
#25437,#25438,#25439,#25440,#25441,#25442,#25443,#25444,#25445,#25446,#25447,
#25448,#25449,#25450,#25451,#25452,#25453,#25454,#25455,#25456,#25457,#25458,
#25459,#25460,#25461,#25462,#25463,#25464,#25465,#25466,#25467,#25468,#25469,
#25470,#25471,#25472,#25473,#25474,#25475,#25476,#25477,#25478,#25479,#25480,
#25481,#25482,#25483,#25484,#25485,#25486,#25487,#25488,#25489,#25490,#25491,
#25492,#25493,#25494,#25495,#25496,#25497,#25498,#25499,#25500,#25501,#25502,
#25503,#25504,#25505,#25506,#25507,#25508,#25509,#25510,#25511,#25512,#25513,
#25514,#25515,#25516,#25517,#25518,#25519,#25520,#25521,#25522,#25523,#25524,
#25525,#25526,#25527,#25528,#25529,#25530,#25531,#25532,#25533,#25534,#25535,
#25536,#25537,#25538,#25539,#25540,#25541,#25542,#25543,#25544,#25545,#25546,
#25547,#25548,#25549,#25550,#25551,#25552,#25553,#25554,#25555,#25556,#25557,
#25558,#25559,#25560,#25561,#25562,#25563,#25564,#25565,#25566,#25567,#25568,
#25569,#25570,#25571,#25572,#25573,#25574,#25575,#25576,#25577,#25578,#25579,
#25580,#25581,#25582,#25583,#25584,#25585,#25586,#25587,#25588,#25589,#25590,
#25591,#25592,#25593,#25594,#25595,#25596,#25597,#25598,#25599,#25600,#25601,
#25602,#25603,#25604,#25605,#25606,#25607,#25608,#25609,#25610,#25611,#25612,
#25613,#25614,#25615,#25616,#25617,#25618,#25619,#25620,#25621,#25622,#25623,
#25624,#25625,#25626,#25627,#25628,#25629,#25630,#25631,#25632,#25633,#25634,
#25635,#25636,#25637,#25638,#25639,#25640,#25641,#25642,#25643,#25644,#25645,
#25646,#25647,#25648,#25649,#25650,#25651,#25652,#25653,#25654,#25655,#25656,
#25657,#25658,#25659,#25660,#25661,#25662,#25663,#25664,#25665,#25666,#25667,
#25668,#25669,#25670,#25671,#25672,#25673,#25674,#25675,#25676,#25677,#25678,
#25679,#25680,#25681,#25682,#25683,#25684,#25685,#25686,#25687,#25688,#25689,
#25690,#25691,#25692,#25693,#25694,#25695,#25696,#25697,#25698,#25699,#25700,
#25701,#25702,#25703,#25704,#25705,#25706,#25707,#25708,#25709,#25710,#25711,
#25712,#25713,#25714,#25715,#25716,#25717,#25718,#25719,#25720,#25721,#25722,
#25723,#25724,#25725,#25726,#25727,#25728,#25729,#25730,#25731,#25732,#25733,
#25734,#25735,#25736,#25737,#25738,#25739,#25740,#25741,#25742,#25743,#25744,
#25745,#25746,#25747,#25748,#25749,#25750,#25751,#25752,#25753,#25754,#25755,
#25756,#25757,#25758,#25759,#25760,#25761,#25762,#25763,#25764,#25765,#25766,
#25767,#25768,#25769,#25770,#25771,#25772,#25773,#25774,#25775,#25776,#25777,
#25778,#25779,#25780,#25781,#25782,#25783,#25784,#25785,#25786,#25787),
(#25788,#25789,#25790,#25791,#25792,#25793,#25794,#25795,#25796,#25797,
#25798,#25799,#25800,#25801,#25802,#25803,#25804,#25805,#25806,#25807,#25808,
#25809,#25810,#25811,#25812,#25813,#25814,#25815,#25816,#25817,#25818,#25819,
#25820,#25821,#25822,#25823,#25824,#25825,#25826,#25827,#25828,#25829,#25830,
#25831,#25832,#25833,#25834,#25835,#25836,#25837,#25838,#25839,#25840,#25841,
#25842,#25843,#25844,#25845,#25846,#25847,#25848,#25849,#25850,#25851,#25852,
#25853,#25854,#25855,#25856,#25857,#25858,#25859,#25860,#25861,#25862,#25863,
#25864,#25865,#25866,#25867,#25868,#25869,#25870,#25871,#25872,#25873,#25874,
#25875,#25876,#25877,#25878,#25879,#25880,#25881,#25882,#25883,#25884,#25885,
#25886,#25887,#25888,#25889,#25890,#25891,#25892,#25893,#25894,#25895,#25896,
#25897,#25898,#25899,#25900,#25901,#25902,#25903,#25904,#25905,#25906,#25907,
#25908,#25909,#25910,#25911,#25912,#25913,#25914,#25915,#25916,#25917,#25918,
#25919,#25920,#25921,#25922,#25923,#25924,#25925,#25926,#25927,#25928,#25929,
#25930,#25931,#25932,#25933,#25934,#25935,#25936,#25937,#25938,#25939,#25940,
#25941,#25942,#25943,#25944,#25945,#25946,#25947,#25948,#25949,#25950,#25951,
#25952,#25953,#25954,#25955,#25956,#25957,#25958,#25959,#25960,#25961,#25962,
#25963,#25964,#25965,#25966,#25967,#25968,#25969,#25970,#25971,#25972,#25973,
#25974,#25975,#25976,#25977,#25978,#25979,#25980,#25981,#25982,#25983,#25984,
#25985,#25986,#25987,#25988,#25989,#25990,#25991,#25992,#25993,#25994,#25995,
#25996,#25997,#25998,#25999,#26000,#26001,#26002,#26003,#26004,#26005,#26006,
#26007,#26008,#26009,#26010,#26011,#26012,#26013,#26014,#26015,#26016,#26017,
#26018,#26019,#26020,#26021,#26022,#26023,#26024,#26025,#26026,#26027,#26028,
#26029,#26030,#26031,#26032,#26033,#26034,#26035,#26036,#26037,#26038,#26039,
#26040,#26041,#26042,#26043,#26044,#26045,#26046,#26047,#26048,#26049,#26050,
#26051,#26052,#26053,#26054,#26055,#26056,#26057,#26058,#26059,#26060,#26061,
#26062,#26063,#26064,#26065,#26066,#26067,#26068,#26069,#26070,#26071,#26072,
#26073,#26074,#26075,#26076,#26077,#26078,#26079,#26080,#26081,#26082,#26083,
#26084,#26085,#26086,#26087,#26088,#26089,#26090,#26091,#26092,#26093,#26094,
#26095,#26096,#26097,#26098,#26099,#26100,#26101,#26102,#26103,#26104,#26105,
#26106,#26107,#26108,#26109,#26110,#26111,#26112,#26113,#26114,#26115,#26116,
#26117,#26118,#26119,#26120,#26121,#26122,#26123,#26124,#26125,#26126,#26127,
#26128,#26129,#26130,#26131,#26132,#26133,#26134,#26135,#26136,#26137,#26138,
#26139,#26140,#26141,#26142,#26143,#26144,#26145,#26146,#26147,#26148,#26149,
#26150,#26151,#26152,#26153,#26154,#26155,#26156,#26157,#26158,#26159,#26160,
#26161,#26162,#26163,#26164,#26165,#26166,#26167,#26168,#26169,#26170,#26171,
#26172,#26173,#26174,#26175,#26176,#26177,#26178,#26179,#26180,#26181,#26182,
#26183,#26184,#26185,#26186,#26187,#26188,#26189,#26190,#26191,#26192,#26193,
#26194,#26195,#26196,#26197,#26198,#26199,#26200,#26201,#26202,#26203,#26204,
#26205,#26206,#26207,#26208,#26209,#26210,#26211,#26212,#26213,#26214,#26215,
#26216,#26217,#26218,#26219,#26220,#26221,#26222,#26223,#26224,#26225,#26226,
#26227,#26228,#26229,#26230,#26231,#26232,#26233,#26234,#26235,#26236,#26237,
#26238,#26239,#26240,#26241,#26242,#26243,#26244),(#26245,#26246,#26247,
#26248,#26249,#26250,#26251,#26252,#26253,#26254,#26255,#26256,#26257,#26258,
#26259,#26260,#26261,#26262,#26263,#26264,#26265,#26266,#26267,#26268,#26269,
#26270,#26271,#26272,#26273,#26274,#26275,#26276,#26277,#26278,#26279,#26280,
#26281,#26282,#26283,#26284,#26285,#26286,#26287,#26288,#26289,#26290,#26291,
#26292,#26293,#26294,#26295,#26296,#26297,#26298,#26299,#26300,#26301,#26302,
#26303,#26304,#26305,#26306,#26307,#26308,#26309,#26310,#26311,#26312,#26313,
#26314,#26315,#26316,#26317,#26318,#26319,#26320,#26321,#26322,#26323,#26324,
#26325,#26326,#26327,#26328,#26329,#26330,#26331,#26332,#26333,#26334,#26335,
#26336,#26337,#26338,#26339,#26340,#26341,#26342,#26343,#26344,#26345,#26346,
#26347,#26348,#26349,#26350,#26351,#26352,#26353,#26354,#26355,#26356,#26357,
#26358,#26359,#26360,#26361,#26362,#26363,#26364,#26365,#26366,#26367,#26368,
#26369,#26370,#26371,#26372,#26373,#26374,#26375,#26376,#26377,#26378,#26379,
#26380,#26381,#26382,#26383,#26384,#26385,#26386,#26387,#26388,#26389,#26390,
#26391,#26392,#26393,#26394,#26395,#26396,#26397,#26398,#26399,#26400,#26401,
#26402,#26403,#26404,#26405,#26406,#26407,#26408,#26409,#26410,#26411,#26412,
#26413,#26414,#26415,#26416,#26417,#26418,#26419,#26420,#26421,#26422,#26423,
#26424,#26425,#26426,#26427,#26428,#26429,#26430,#26431,#26432,#26433,#26434,
#26435,#26436,#26437,#26438,#26439,#26440,#26441,#26442,#26443,#26444,#26445,
#26446,#26447,#26448,#26449,#26450,#26451,#26452,#26453,#26454,#26455,#26456,
#26457,#26458,#26459,#26460,#26461,#26462,#26463,#26464,#26465,#26466,#26467,
#26468,#26469,#26470,#26471,#26472,#26473,#26474,#26475,#26476,#26477,#26478,
#26479,#26480,#26481,#26482,#26483,#26484,#26485,#26486,#26487,#26488,#26489,
#26490,#26491,#26492,#26493,#26494,#26495,#26496,#26497,#26498,#26499,#26500,
#26501,#26502,#26503,#26504,#26505,#26506,#26507,#26508,#26509,#26510,#26511,
#26512,#26513,#26514,#26515,#26516,#26517,#26518,#26519,#26520,#26521,#26522,
#26523,#26524,#26525,#26526,#26527,#26528,#26529,#26530,#26531,#26532,#26533,
#26534,#26535,#26536,#26537,#26538,#26539,#26540,#26541,#26542,#26543,#26544,
#26545,#26546,#26547,#26548,#26549,#26550,#26551,#26552,#26553,#26554,#26555,
#26556,#26557,#26558,#26559,#26560,#26561,#26562,#26563,#26564,#26565,#26566,
#26567,#26568,#26569,#26570,#26571,#26572,#26573,#26574,#26575,#26576,#26577,
#26578,#26579,#26580,#26581,#26582,#26583,#26584,#26585,#26586,#26587,#26588,
#26589,#26590,#26591,#26592,#26593,#26594,#26595,#26596,#26597,#26598,#26599,
#26600,#26601,#26602,#26603,#26604,#26605,#26606,#26607,#26608,#26609,#26610,
#26611,#26612,#26613,#26614,#26615,#26616,#26617,#26618,#26619,#26620,#26621,
#26622,#26623,#26624,#26625,#26626,#26627,#26628,#26629,#26630,#26631,#26632,
#26633,#26634,#26635,#26636,#26637,#26638,#26639,#26640,#26641,#26642,#26643,
#26644,#26645,#26646,#26647,#26648,#26649,#26650,#26651,#26652,#26653,#26654,
#26655,#26656,#26657,#26658,#26659,#26660,#26661,#26662,#26663,#26664,#26665,
#26666,#26667,#26668,#26669,#26670,#26671,#26672,#26673,#26674,#26675,#26676,
#26677,#26678,#26679,#26680,#26681,#26682,#26683,#26684,#26685,#26686,#26687,
#26688,#26689,#26690,#26691,#26692,#26693,#26694,#26695,#26696,#26697,#26698,
#26699,#26700,#26701),(#26702,#26703,#26704,#26705,#26706,#26707,#26708,
#26709,#26710,#26711,#26712,#26713,#26714,#26715,#26716,#26717,#26718,#26719,
#26720,#26721,#26722,#26723,#26724,#26725,#26726,#26727,#26728,#26729,#26730,
#26731,#26732,#26733,#26734,#26735,#26736,#26737,#26738,#26739,#26740,#26741,
#26742,#26743,#26744,#26745,#26746,#26747,#26748,#26749,#26750,#26751,#26752,
#26753,#26754,#26755,#26756,#26757,#26758,#26759,#26760,#26761,#26762,#26763,
#26764,#26765,#26766,#26767,#26768,#26769,#26770,#26771,#26772,#26773,#26774,
#26775,#26776,#26777,#26778,#26779,#26780,#26781,#26782,#26783,#26784,#26785,
#26786,#26787,#26788,#26789,#26790,#26791,#26792,#26793,#26794,#26795,#26796,
#26797,#26798,#26799,#26800,#26801,#26802,#26803,#26804,#26805,#26806,#26807,
#26808,#26809,#26810,#26811,#26812,#26813,#26814,#26815,#26816,#26817,#26818,
#26819,#26820,#26821,#26822,#26823,#26824,#26825,#26826,#26827,#26828,#26829,
#26830,#26831,#26832,#26833,#26834,#26835,#26836,#26837,#26838,#26839,#26840,
#26841,#26842,#26843,#26844,#26845,#26846,#26847,#26848,#26849,#26850,#26851,
#26852,#26853,#26854,#26855,#26856,#26857,#26858,#26859,#26860,#26861,#26862,
#26863,#26864,#26865,#26866,#26867,#26868,#26869,#26870,#26871,#26872,#26873,
#26874,#26875,#26876,#26877,#26878,#26879,#26880,#26881,#26882,#26883,#26884,
#26885,#26886,#26887,#26888,#26889,#26890,#26891,#26892,#26893,#26894,#26895,
#26896,#26897,#26898,#26899,#26900,#26901,#26902,#26903,#26904,#26905,#26906,
#26907,#26908,#26909,#26910,#26911,#26912,#26913,#26914,#26915,#26916,#26917,
#26918,#26919,#26920,#26921,#26922,#26923,#26924,#26925,#26926,#26927,#26928,
#26929,#26930,#26931,#26932,#26933,#26934,#26935,#26936,#26937,#26938,#26939,
#26940,#26941,#26942,#26943,#26944,#26945,#26946,#26947,#26948,#26949,#26950,
#26951,#26952,#26953,#26954,#26955,#26956,#26957,#26958,#26959,#26960,#26961,
#26962,#26963,#26964,#26965,#26966,#26967,#26968,#26969,#26970,#26971,#26972,
#26973,#26974,#26975,#26976,#26977,#26978,#26979,#26980,#26981,#26982,#26983,
#26984,#26985,#26986,#26987,#26988,#26989,#26990,#26991,#26992,#26993,#26994,
#26995,#26996,#26997,#26998,#26999,#27000,#27001,#27002,#27003,#27004,#27005,
#27006,#27007,#27008,#27009,#27010,#27011,#27012,#27013,#27014,#27015,#27016,
#27017,#27018,#27019,#27020,#27021,#27022,#27023,#27024,#27025,#27026,#27027,
#27028,#27029,#27030,#27031,#27032,#27033,#27034,#27035,#27036,#27037,#27038,
#27039,#27040,#27041,#27042,#27043,#27044,#27045,#27046,#27047,#27048,#27049,
#27050,#27051,#27052,#27053,#27054,#27055,#27056,#27057,#27058,#27059,#27060,
#27061,#27062,#27063,#27064,#27065,#27066,#27067,#27068,#27069,#27070,#27071,
#27072,#27073,#27074,#27075,#27076,#27077,#27078,#27079,#27080,#27081,#27082,
#27083,#27084,#27085,#27086,#27087,#27088,#27089,#27090,#27091,#27092,#27093,
#27094,#27095,#27096,#27097,#27098,#27099,#27100,#27101,#27102,#27103,#27104,
#27105,#27106,#27107,#27108,#27109,#27110,#27111,#27112,#27113,#27114,#27115,
#27116,#27117,#27118,#27119,#27120,#27121,#27122,#27123,#27124,#27125,#27126,
#27127,#27128,#27129,#27130,#27131,#27132,#27133,#27134,#27135,#27136,#27137,
#27138,#27139,#27140,#27141,#27142,#27143,#27144,#27145,#27146,#27147,#27148,
#27149,#27150,#27151,#27152,#27153,#27154,#27155,#27156,#27157,#27158)),
 .UNSPECIFIED.,.T.,.F.,.F.)
B_SPLINE_SURFACE_WITH_KNOTS((4,3,4),(3,2,2,2,2,2,2,2,2,2,2,2,2,2,2,2,2,
2,2,2,2,2,2,2,2,2,2,2,2,2,2,2,2,2,2,2,2,2,2,2,2,2,2,2,2,2,2,2,2,2,2,2,2,
2,2,2,2,2,2,2,2,2,2,2,2,2,2,2,2,2,2,2,2,2,2,2,2,2,2,2,2,2,2,2,2,2,2,2,2,
2,2,2,2,2,2,2,2,2,2,2,2,2,2,2,2,2,2,2,2,2,2,2,2,2,2,2,2,2,2,2,2,2,2,2,2,
2,2,2,2,2,2,2,2,2,2,2,2,2,2,2,2,2,2,2,2,2,2,2,2,2,2,2,2,2,2,2,2,2,2,2,2,
2,2,2,2,2,2,2,2,2,2,2,2,2,2,2,2,2,2,2,2,2,2,2,2,2,2,2,2,2,2,2,2,2,2,2,2,
2,2,2,2,2,2,2,2,2,2,2,2,2,2,2,2,2,2,2,2,2,2,2,2,2,2,2,2,2,2,2,3),(0.,0.5,
1.),(0.,0.0043859649122807,0.0087719298245614,0.0131578947368421,0.0175438596491228,
0.0219298245614035,0.0263157894736842,0.0307017543859649,0.0350877192982456,
0.0394736842105263,0.043859649122807,0.0482456140350877,0.0526315789473684,
0.0570175438596491,0.0614035087719298,0.0657894736842105,0.0701754385964912,
0.0745614035087719,0.0789473684210526,0.0833333333333333,0.087719298245614,
0.0921052631578947,0.0964912280701754,0.100877192982456,0.105263157894737,
0.109649122807018,0.114035087719298,0.118421052631579,0.12280701754386,
0.12719298245614,0.131578947368421,0.135964912280702,0.140350877192982,
0.144736842105263,0.149122807017544,0.153508771929825,0.157894736842105,
0.162280701754386,0.166666666666667,0.171052631578947,0.175438596491228,
0.179824561403509,0.184210526315789,0.18859649122807,0.192982456140351,
0.197368421052632,0.201754385964912,0.206140350877193,0.210526315789474,
0.214912280701754,0.219298245614035,0.223684210526316,0.228070175438596,
0.232456140350877,0.236842105263158,0.241228070175439,0.245614035087719,
0.25,0.254385964912281,0.258771929824561,0.263157894736842,0.267543859649123,
0.271929824561404,0.276315789473684,0.280701754385965,0.285087719298246,
0.289473684210526,0.293859649122807,0.298245614035088,0.302631578947368,
0.307017543859649,0.31140350877193,0.315789473684211,0.320175438596491,
0.324561403508772,0.328947368421053,0.333333333333333,0.337719298245614,
0.342105263157895,0.346491228070175,0.350877192982456,0.355263157894737,
0.359649122807018,0.364035087719298,0.368421052631579,0.37280701754386,
0.37719298245614,0.381578947368421,0.385964912280702,0.390350877192982,
0.394736842105263,0.399122807017544,0.403508771929825,0.407894736842105,
0.412280701754386,0.416666666666667,0.421052631578947,0.425438596491228,
0.429824561403509,0.434210526315789,0.43859649122807,0.442982456140351,
0.447368421052632,0.451754385964912,0.456140350877193,0.460526315789474,
0.464912280701754,0.469298245614035,0.473684210526316,0.478070175438596,
0.482456140350877,0.486842105263158,0.491228070175439,0.495614035087719,
0.5,0.504385964912281,0.508771929824561,0.513157894736842,0.517543859649123,
0.521929824561403,0.526315789473684,0.530701754385965,0.535087719298246,
0.539473684210526,0.543859649122807,0.548245614035088,0.552631578947368,
0.557017543859649,0.56140350877193,0.565789473684211,0.570175438596491,
0.574561403508772,0.578947368421053,0.583333333333333,0.587719298245614,
0.592105263157895,0.596491228070175,0.600877192982456,0.605263157894737,
0.609649122807018,0.614035087719298,0.618421052631579,0.62280701754386,
0.62719298245614,0.631578947368421,0.635964912280702,0.640350877192982,
0.644736842105263,0.649122807017544,0.653508771929825,0.657894736842105,
0.662280701754386,0.666666666666667,0.671052631578947,0.675438596491228,
0.679824561403509,0.684210526315789,0.68859649122807,0.692982456140351,
0.697368421052632,0.701754385964912,0.706140350877193,0.710526315789474,
0.714912280701754,0.719298245614035,0.723684210526316,0.728070175438597,
0.732456140350877,0.736842105263158,0.741228070175439,0.745614035087719,
0.75,0.754385964912281,0.758771929824561,0.763157894736842,0.767543859649123,
0.771929824561403,0.776315789473684,0.780701754385965,0.785087719298246,
0.789473684210526,0.793859649122807,0.798245614035088,0.802631578947368,
0.807017543859649,0.81140350877193,0.815789473684211,0.820175438596491,
0.824561403508772,0.828947368421053,0.833333333333333,0.837719298245614,
0.842105263157895,0.846491228070175,0.850877192982456,0.855263157894737,
0.859649122807018,0.864035087719298,0.868421052631579,0.87280701754386,
0.87719298245614,0.881578947368421,0.885964912280702,0.890350877192982,
0.894736842105263,0.899122807017544,0.903508771929825,0.907894736842105,
0.912280701754386,0.916666666666667,0.921052631578947,0.925438596491228,
0.929824561403509,0.934210526315789,0.93859649122807,0.942982456140351,
0.947368421052632,0.951754385964912,0.956140350877193,0.960526315789474,
0.964912280701754,0.969298245614035,0.973684210526316,0.978070175438597,
0.982456140350877,0.986842105263158,0.991228070175439,0.995614035087719,
1.),.UNSPECIFIED.)
GEOMETRIC_REPRESENTATION_ITEM()
RATIONAL_B_SPLINE_SURFACE(((1.,0.965925826289068,1.,0.965925826289068,1.,
0.965925826289068,1.,0.965925826289068,1.,0.965925826289068,1.,0.965925826289068,
1.,0.965925826289068,1.,0.965925826289068,1.,0.965925826289068,1.,0.965925826289068,
1.,0.965925826289068,1.,0.965925826289068,1.,0.965925826289068,1.,0.965925826289068,
1.,0.965925826289068,1.,0.965925826289068,1.,0.965925826289068,1.,0.965925826289068,
1.,0.965925826289068,1.,0.965925826289068,1.,0.965925826289068,1.,0.965925826289068,
1.,0.965925826289068,1.,0.965925826289068,1.,0.965925826289068,1.,0.965925826289068,
1.,0.965925826289068,1.,0.965925826289068,1.,0.965925826289068,1.,0.965925826289068,
1.,0.965925826289068,1.,0.965925826289068,1.,0.965925826289068,1.,0.965925826289068,
1.,0.965925826289068,1.,0.965925826289068,1.,0.965925826289068,1.,0.965925826289068,
1.,0.965925826289068,1.,0.965925826289068,1.,0.965925826289068,1.,0.965925826289068,
1.,0.965925826289068,1.,0.965925826289068,1.,0.965925826289068,1.,0.965925826289068,
1.,0.965925826289068,1.,0.965925826289068,1.,0.965925826289068,1.,0.965925826289068,
1.,0.965925826289068,1.,0.965925826289068,1.,0.965925826289068,1.,0.965925826289068,
1.,0.965925826289068,1.,0.965925826289068,1.,0.965925826289068,1.,0.965925826289068,
1.,0.965925826289068,1.,0.965925826289068,1.,0.965925826289068,1.,0.965925826289068,
1.,0.965925826289068,1.,0.965925826289068,1.,0.965925826289068,1.,0.965925826289068,
1.,0.965925826289068,1.,0.965925826289068,1.,0.965925826289068,1.,0.965925826289068,
1.,0.965925826289068,1.,0.965925826289068,1.,0.965925826289068,1.,0.965925826289068,
1.,0.965925826289068,1.,0.965925826289068,1.,0.965925826289068,1.,0.965925826289068,
1.,0.965925826289068,1.,0.965925826289068,1.,0.965925826289068,1.,0.965925826289068,
1.,0.965925826289068,1.,0.965925826289068,1.,0.965925826289068,1.,0.965925826289068,
1.,0.965925826289068,1.,0.965925826289068,1.,0.965925826289068,1.,0.965925826289068,
1.,0.965925826289068,1.,0.965925826289068,1.,0.965925826289068,1.,0.965925826289068,
1.,0.965925826289068,1.,0.965925826289068,1.,0.965925826289068,1.,0.965925826289068,
1.,0.965925826289068,1.,0.965925826289068,1.,0.965925826289068,1.,0.965925826289068,
1.,0.965925826289068,1.,0.965925826289068,1.,0.965925826289068,1.,0.965925826289068,
1.,0.965925826289068,1.,0.965925826289068,1.,0.965925826289068,1.,0.965925826289068,
1.,0.965925826289068,1.,0.965925826289068,1.,0.965925826289068,1.,0.965925826289068,
1.,0.965925826289068,1.,0.965925826289068,1.,0.965925826289068,1.,0.965925826289068,
1.,0.965925826289068,1.,0.965925826289068,1.,0.965925826289068,1.,0.965925826289068,
1.,0.965925826289068,1.,0.965925826289068,1.,0.965925826289068,1.,0.965925826289068,
1.,0.965925826289068,1.,0.965925826289068,1.,0.965925826289068,1.,0.965925826289068,
1.,0.965925826289068,1.,0.965925826289068,1.,0.965925826289068,1.,0.965925826289068,
1.,0.965925826289068,1.,0.965925826289068,1.,0.965925826289068,1.,0.965925826289068,
1.,0.965925826289068,1.,0.965925826289068,1.,0.965925826289068,1.,0.965925826289068,
1.,0.965925826289068,1.,0.965925826289068,1.,0.965925826289068,1.,0.965925826289068,
1.,0.965925826289068,1.,0.965925826289068,1.,0.965925826289068,1.,0.965925826289068,
1.,0.965925826289068,1.,0.965925826289068,1.,0.965925826289068,1.,0.965925826289068,
1.,0.965925826289068,1.,0.965925826289068,1.,0.965925826289068,1.,0.965925826289068,
1.,0.965925826289068,1.,0.965925826289068,1.,0.965925826289068,1.,0.965925826289068,
1.,0.965925826289068,1.,0.965925826289068,1.,0.965925826289068,1.,0.965925826289068,
1.,0.965925826289068,1.,0.965925826289068,1.,0.965925826289068,1.,0.965925826289068,
1.,0.965925826289068,1.,0.965925826289068,1.,0.965925826289068,1.,0.965925826289068,
1.,0.965925826289068,1.,0.965925826289068,1.,0.965925826289068,1.,0.965925826289068,
1.,0.965925826289068,1.,0.965925826289068,1.,0.965925826289068,1.,0.965925826289068,
1.,0.965925826289068,1.,0.965925826289068,1.,0.965925826289068,1.,0.965925826289068,
1.,0.965925826289068,1.,0.965925826289068,1.,0.965925826289068,1.,0.965925826289068,
1.,0.965925826289068,1.,0.965925826289068,1.,0.965925826289068,1.,0.965925826289068,
1.,0.965925826289068,1.,0.965925826289068,1.,0.965925826289068,1.,0.965925826289068,
1.,0.965925826289068,1.,0.965925826289068,1.,0.965925826289068,1.,0.965925826289068,
1.,0.965925826289068,1.,0.965925826289068,1.,0.965925826289068,1.,0.965925826289068,
1.,0.965925826289068,1.,0.965925826289068,1.,0.965925826289068,1.,0.965925826289068,
1.,0.965925826289068,1.,0.965925826289068,1.,0.965925826289068,1.,0.965925826289068,
1.,0.965925826289068,1.,0.965925826289068,1.,0.965925826289068,1.,0.965925826289068,
1.,0.965925826289068,1.,0.965925826289068,1.,0.965925826289068,1.,0.965925826289068,
1.,0.965925826289068,1.,0.965925826289068,1.,0.965925826289068,1.,0.965925826289068,
1.,0.965925826289068,1.,0.965925826289068,1.),(0.333333333333333,0.321975275429689,
0.333333333333333,0.321975275429689,0.333333333333333,0.321975275429689,
0.333333333333333,0.321975275429689,0.333333333333333,0.321975275429689,
0.333333333333333,0.321975275429689,0.333333333333333,0.321975275429689,
0.333333333333333,0.321975275429689,0.333333333333333,0.321975275429689,
0.333333333333333,0.321975275429689,0.333333333333333,0.321975275429689,
0.333333333333333,0.321975275429689,0.333333333333333,0.321975275429689,
0.333333333333333,0.321975275429689,0.333333333333333,0.321975275429689,
0.333333333333333,0.321975275429689,0.333333333333333,0.321975275429689,
0.333333333333333,0.321975275429689,0.333333333333333,0.321975275429689,
0.333333333333333,0.321975275429689,0.333333333333333,0.321975275429689,
0.333333333333333,0.321975275429689,0.333333333333333,0.321975275429689,
0.333333333333333,0.321975275429689,0.333333333333333,0.321975275429689,
0.333333333333333,0.321975275429689,0.333333333333333,0.321975275429689,
0.333333333333333,0.321975275429689,0.333333333333333,0.321975275429689,
0.333333333333333,0.321975275429689,0.333333333333333,0.321975275429689,
0.333333333333333,0.321975275429689,0.333333333333333,0.321975275429689,
0.333333333333333,0.321975275429689,0.333333333333333,0.321975275429689,
0.333333333333333,0.321975275429689,0.333333333333333,0.321975275429689,
0.333333333333333,0.321975275429689,0.333333333333333,0.321975275429689,
0.333333333333333,0.321975275429689,0.333333333333333,0.321975275429689,
0.333333333333333,0.321975275429689,0.333333333333333,0.321975275429689,
0.333333333333333,0.321975275429689,0.333333333333333,0.321975275429689,
0.333333333333333,0.321975275429689,0.333333333333333,0.321975275429689,
0.333333333333333,0.321975275429689,0.333333333333333,0.321975275429689,
0.333333333333333,0.321975275429689,0.333333333333333,0.321975275429689,
0.333333333333333,0.321975275429689,0.333333333333333,0.321975275429689,
0.333333333333333,0.321975275429689,0.333333333333333,0.321975275429689,
0.333333333333333,0.321975275429689,0.333333333333333,0.321975275429689,
0.333333333333333,0.321975275429689,0.333333333333333,0.321975275429689,
0.333333333333333,0.321975275429689,0.333333333333333,0.321975275429689,
0.333333333333333,0.321975275429689,0.333333333333333,0.321975275429689,
0.333333333333333,0.321975275429689,0.333333333333333,0.321975275429689,
0.333333333333333,0.321975275429689,0.333333333333333,0.321975275429689,
0.333333333333333,0.321975275429689,0.333333333333333,0.321975275429689,
0.333333333333333,0.321975275429689,0.333333333333333,0.321975275429689,
0.333333333333333,0.321975275429689,0.333333333333333,0.321975275429689,
0.333333333333333,0.321975275429689,0.333333333333333,0.321975275429689,
0.333333333333333,0.321975275429689,0.333333333333333,0.321975275429689,
0.333333333333333,0.321975275429689,0.333333333333333,0.321975275429689,
0.333333333333333,0.321975275429689,0.333333333333333,0.321975275429689,
0.333333333333333,0.321975275429689,0.333333333333333,0.321975275429689,
0.333333333333333,0.321975275429689,0.333333333333333,0.321975275429689,
0.333333333333333,0.321975275429689,0.333333333333333,0.321975275429689,
0.333333333333333,0.321975275429689,0.333333333333333,0.321975275429689,
0.333333333333333,0.321975275429689,0.333333333333333,0.321975275429689,
0.333333333333333,0.321975275429689,0.333333333333333,0.321975275429689,
0.333333333333333,0.321975275429689,0.333333333333333,0.321975275429689,
0.333333333333333,0.321975275429689,0.333333333333333,0.321975275429689,
0.333333333333333,0.321975275429689,0.333333333333333,0.321975275429689,
0.333333333333333,0.321975275429689,0.333333333333333,0.321975275429689,
0.333333333333333,0.321975275429689,0.333333333333333,0.321975275429689,
0.333333333333333,0.321975275429689,0.333333333333333,0.321975275429689,
0.333333333333333,0.321975275429689,0.333333333333333,0.321975275429689,
0.333333333333333,0.321975275429689,0.333333333333333,0.321975275429689,
0.333333333333333,0.321975275429689,0.333333333333333,0.321975275429689,
0.333333333333333,0.321975275429689,0.333333333333333,0.321975275429689,
0.333333333333333,0.321975275429689,0.333333333333333,0.321975275429689,
0.333333333333333,0.321975275429689,0.333333333333333,0.321975275429689,
0.333333333333333,0.321975275429689,0.333333333333333,0.321975275429689,
0.333333333333333,0.321975275429689,0.333333333333333,0.321975275429689,
0.333333333333333,0.321975275429689,0.333333333333333,0.321975275429689,
0.333333333333333,0.321975275429689,0.333333333333333,0.321975275429689,
0.333333333333333,0.321975275429689,0.333333333333333,0.321975275429689,
0.333333333333333,0.321975275429689,0.333333333333333,0.321975275429689,
0.333333333333333,0.321975275429689,0.333333333333333,0.321975275429689,
0.333333333333333,0.321975275429689,0.333333333333333,0.321975275429689,
0.333333333333333,0.321975275429689,0.333333333333333,0.321975275429689,
0.333333333333333,0.321975275429689,0.333333333333333,0.321975275429689,
0.333333333333333,0.321975275429689,0.333333333333333,0.321975275429689,
0.333333333333333,0.321975275429689,0.333333333333333,0.321975275429689,
0.333333333333333,0.321975275429689,0.333333333333333,0.321975275429689,
0.333333333333333,0.321975275429689,0.333333333333333,0.321975275429689,
0.333333333333333,0.321975275429689,0.333333333333333,0.321975275429689,
0.333333333333333,0.321975275429689,0.333333333333333,0.321975275429689,
0.333333333333333,0.321975275429689,0.333333333333333,0.321975275429689,
0.333333333333333,0.321975275429689,0.333333333333333,0.321975275429689,
0.333333333333333,0.321975275429689,0.333333333333333,0.321975275429689,
0.333333333333333,0.321975275429689,0.333333333333333,0.321975275429689,
0.333333333333333,0.321975275429689,0.333333333333333,0.321975275429689,
0.333333333333333,0.321975275429689,0.333333333333333,0.321975275429689,
0.333333333333333,0.321975275429689,0.333333333333333,0.321975275429689,
0.333333333333333,0.321975275429689,0.333333333333333,0.321975275429689,
0.333333333333333,0.321975275429689,0.333333333333333,0.321975275429689,
0.333333333333333,0.321975275429689,0.333333333333333,0.321975275429689,
0.333333333333333,0.321975275429689,0.333333333333333,0.321975275429689,
0.333333333333333,0.321975275429689,0.333333333333333,0.321975275429689,
0.333333333333333,0.321975275429689,0.333333333333333,0.321975275429689,
0.333333333333333,0.321975275429689,0.333333333333333,0.321975275429689,
0.333333333333333,0.321975275429689,0.333333333333333,0.321975275429689,
0.333333333333333,0.321975275429689,0.333333333333333,0.321975275429689,
0.333333333333333,0.321975275429689,0.333333333333333,0.321975275429689,
0.333333333333333,0.321975275429689,0.333333333333333,0.321975275429689,
0.333333333333333,0.321975275429689,0.333333333333333,0.321975275429689,
0.333333333333333,0.321975275429689,0.333333333333333,0.321975275429689,
0.333333333333333,0.321975275429689,0.333333333333333,0.321975275429689,
0.333333333333333,0.321975275429689,0.333333333333333,0.321975275429689,
0.333333333333333,0.321975275429689,0.333333333333333,0.321975275429689,
0.333333333333333,0.321975275429689,0.333333333333333,0.321975275429689,
0.333333333333333,0.321975275429689,0.333333333333333,0.321975275429689,
0.333333333333333,0.321975275429689,0.333333333333333,0.321975275429689,
0.333333333333333,0.321975275429689,0.333333333333333,0.321975275429689,
0.333333333333333,0.321975275429689,0.333333333333333,0.321975275429689,
0.333333333333333,0.321975275429689,0.333333333333333,0.321975275429689,
0.333333333333333,0.321975275429689,0.333333333333333,0.321975275429689,
0.333333333333333,0.321975275429689,0.333333333333333,0.321975275429689,
0.333333333333333,0.321975275429689,0.333333333333333,0.321975275429689,
0.333333333333333,0.321975275429689,0.333333333333333,0.321975275429689,
0.333333333333333,0.321975275429689,0.333333333333333,0.321975275429689,
0.333333333333333,0.321975275429689,0.333333333333333,0.321975275429689,
0.333333333333333,0.321975275429689,0.333333333333333,0.321975275429689,
0.333333333333333,0.321975275429689,0.333333333333333,0.321975275429689,
0.333333333333333,0.321975275429689,0.333333333333333,0.321975275429689,
0.333333333333333,0.321975275429689,0.333333333333333,0.321975275429689,
0.333333333333333,0.321975275429689,0.333333333333333),(0.333333333333333,
0.321975275429689,0.333333333333333,0.321975275429689,0.333333333333333,
0.321975275429689,0.333333333333333,0.321975275429689,0.333333333333333,
0.321975275429689,0.333333333333333,0.321975275429689,0.333333333333333,
0.321975275429689,0.333333333333333,0.321975275429689,0.333333333333333,
0.321975275429689,0.333333333333333,0.321975275429689,0.333333333333333,
0.321975275429689,0.333333333333333,0.321975275429689,0.333333333333333,
0.321975275429689,0.333333333333333,0.321975275429689,0.333333333333333,
0.321975275429689,0.333333333333333,0.321975275429689,0.333333333333333,
0.321975275429689,0.333333333333333,0.321975275429689,0.333333333333333,
0.321975275429689,0.333333333333333,0.321975275429689,0.333333333333333,
0.321975275429689,0.333333333333333,0.321975275429689,0.333333333333333,
0.321975275429689,0.333333333333333,0.321975275429689,0.333333333333333,
0.321975275429689,0.333333333333333,0.321975275429689,0.333333333333333,
0.321975275429689,0.333333333333333,0.321975275429689,0.333333333333333,
0.321975275429689,0.333333333333333,0.321975275429689,0.333333333333333,
0.321975275429689,0.333333333333333,0.321975275429689,0.333333333333333,
0.321975275429689,0.333333333333333,0.321975275429689,0.333333333333333,
0.321975275429689,0.333333333333333,0.321975275429689,0.333333333333333,
0.321975275429689,0.333333333333333,0.321975275429689,0.333333333333333,
0.321975275429689,0.333333333333333,0.321975275429689,0.333333333333333,
0.321975275429689,0.333333333333333,0.321975275429689,0.333333333333333,
0.321975275429689,0.333333333333333,0.321975275429689,0.333333333333333,
0.321975275429689,0.333333333333333,0.321975275429689,0.333333333333333,
0.321975275429689,0.333333333333333,0.321975275429689,0.333333333333333,
0.321975275429689,0.333333333333333,0.321975275429689,0.333333333333333,
0.321975275429689,0.333333333333333,0.321975275429689,0.333333333333333,
0.321975275429689,0.333333333333333,0.321975275429689,0.333333333333333,
0.321975275429689,0.333333333333333,0.321975275429689,0.333333333333333,
0.321975275429689,0.333333333333333,0.321975275429689,0.333333333333333,
0.321975275429689,0.333333333333333,0.321975275429689,0.333333333333333,
0.321975275429689,0.333333333333333,0.321975275429689,0.333333333333333,
0.321975275429689,0.333333333333333,0.321975275429689,0.333333333333333,
0.321975275429689,0.333333333333333,0.321975275429689,0.333333333333333,
0.321975275429689,0.333333333333333,0.321975275429689,0.333333333333333,
0.321975275429689,0.333333333333333,0.321975275429689,0.333333333333333,
0.321975275429689,0.333333333333333,0.321975275429689,0.333333333333333,
0.321975275429689,0.333333333333333,0.321975275429689,0.333333333333333,
0.321975275429689,0.333333333333333,0.321975275429689,0.333333333333333,
0.321975275429689,0.333333333333333,0.321975275429689,0.333333333333333,
0.321975275429689,0.333333333333333,0.321975275429689,0.333333333333333,
0.321975275429689,0.333333333333333,0.321975275429689,0.333333333333333,
0.321975275429689,0.333333333333333,0.321975275429689,0.333333333333333,
0.321975275429689,0.333333333333333,0.321975275429689,0.333333333333333,
0.321975275429689,0.333333333333333,0.321975275429689,0.333333333333333,
0.321975275429689,0.333333333333333,0.321975275429689,0.333333333333333,
0.321975275429689,0.333333333333333,0.321975275429689,0.333333333333333,
0.321975275429689,0.333333333333333,0.321975275429689,0.333333333333333,
0.321975275429689,0.333333333333333,0.321975275429689,0.333333333333333,
0.321975275429689,0.333333333333333,0.321975275429689,0.333333333333333,
0.321975275429689,0.333333333333333,0.321975275429689,0.333333333333333,
0.321975275429689,0.333333333333333,0.321975275429689,0.333333333333333,
0.321975275429689,0.333333333333333,0.321975275429689,0.333333333333333,
0.321975275429689,0.333333333333333,0.321975275429689,0.333333333333333,
0.321975275429689,0.333333333333333,0.321975275429689,0.333333333333333,
0.321975275429689,0.333333333333333,0.321975275429689,0.333333333333333,
0.321975275429689,0.333333333333333,0.321975275429689,0.333333333333333,
0.321975275429689,0.333333333333333,0.321975275429689,0.333333333333333,
0.321975275429689,0.333333333333333,0.321975275429689,0.333333333333333,
0.321975275429689,0.333333333333333,0.321975275429689,0.333333333333333,
0.321975275429689,0.333333333333333,0.321975275429689,0.333333333333333,
0.321975275429689,0.333333333333333,0.321975275429689,0.333333333333333,
0.321975275429689,0.333333333333333,0.321975275429689,0.333333333333333,
0.321975275429689,0.333333333333333,0.321975275429689,0.333333333333333,
0.321975275429689,0.333333333333333,0.321975275429689,0.333333333333333,
0.321975275429689,0.333333333333333,0.321975275429689,0.333333333333333,
0.321975275429689,0.333333333333333,0.321975275429689,0.333333333333333,
0.321975275429689,0.333333333333333,0.321975275429689,0.333333333333333,
0.321975275429689,0.333333333333333,0.321975275429689,0.333333333333333,
0.321975275429689,0.333333333333333,0.321975275429689,0.333333333333333,
0.321975275429689,0.333333333333333,0.321975275429689,0.333333333333333,
0.321975275429689,0.333333333333333,0.321975275429689,0.333333333333333,
0.321975275429689,0.333333333333333,0.321975275429689,0.333333333333333,
0.321975275429689,0.333333333333333,0.321975275429689,0.333333333333333,
0.321975275429689,0.333333333333333,0.321975275429689,0.333333333333333,
0.321975275429689,0.333333333333333,0.321975275429689,0.333333333333333,
0.321975275429689,0.333333333333333,0.321975275429689,0.333333333333333,
0.321975275429689,0.333333333333333,0.321975275429689,0.333333333333333,
0.321975275429689,0.333333333333333,0.321975275429689,0.333333333333333,
0.321975275429689,0.333333333333333,0.321975275429689,0.333333333333333,
0.321975275429689,0.333333333333333,0.321975275429689,0.333333333333333,
0.321975275429689,0.333333333333333,0.321975275429689,0.333333333333333,
0.321975275429689,0.333333333333333,0.321975275429689,0.333333333333333,
0.321975275429689,0.333333333333333,0.321975275429689,0.333333333333333,
0.321975275429689,0.333333333333333,0.321975275429689,0.333333333333333,
0.321975275429689,0.333333333333333,0.321975275429689,0.333333333333333,
0.321975275429689,0.333333333333333,0.321975275429689,0.333333333333333,
0.321975275429689,0.333333333333333,0.321975275429689,0.333333333333333,
0.321975275429689,0.333333333333333,0.321975275429689,0.333333333333333,
0.321975275429689,0.333333333333333,0.321975275429689,0.333333333333333,
0.321975275429689,0.333333333333333,0.321975275429689,0.333333333333333,
0.321975275429689,0.333333333333333,0.321975275429689,0.333333333333333,
0.321975275429689,0.333333333333333,0.321975275429689,0.333333333333333,
0.321975275429689,0.333333333333333,0.321975275429689,0.333333333333333,
0.321975275429689,0.333333333333333,0.321975275429689,0.333333333333333,
0.321975275429689,0.333333333333333,0.321975275429689,0.333333333333333,
0.321975275429689,0.333333333333333,0.321975275429689,0.333333333333333,
0.321975275429689,0.333333333333333,0.321975275429689,0.333333333333333,
0.321975275429689,0.333333333333333,0.321975275429689,0.333333333333333,
0.321975275429689,0.333333333333333,0.321975275429689,0.333333333333333,
0.321975275429689,0.333333333333333,0.321975275429689,0.333333333333333,
0.321975275429689,0.333333333333333,0.321975275429689,0.333333333333333,
0.321975275429689,0.333333333333333,0.321975275429689,0.333333333333333,
0.321975275429689,0.333333333333333,0.321975275429689,0.333333333333333,
0.321975275429689,0.333333333333333,0.321975275429689,0.333333333333333,
0.321975275429689,0.333333333333333,0.321975275429689,0.333333333333333,
0.321975275429689,0.333333333333333,0.321975275429689,0.333333333333333,
0.321975275429689,0.333333333333333,0.321975275429689,0.333333333333333,
0.321975275429689,0.333333333333333,0.321975275429689,0.333333333333333,
0.321975275429689,0.333333333333333,0.321975275429689,0.333333333333333,
0.321975275429689,0.333333333333333,0.321975275429689,0.333333333333333,
0.321975275429689,0.333333333333333,0.321975275429689,0.333333333333333,
0.321975275429689,0.333333333333333,0.321975275429689,0.333333333333333,
0.321975275429689,0.333333333333333,0.321975275429689,0.333333333333333,
0.321975275429689,0.333333333333333,0.321975275429689,0.333333333333333),
(1.,0.965925826289068,1.,0.965925826289068,1.,0.965925826289068,1.,0.965925826289068,
1.,0.965925826289068,1.,0.965925826289068,1.,0.965925826289068,1.,0.965925826289068,
1.,0.965925826289068,1.,0.965925826289068,1.,0.965925826289068,1.,0.965925826289068,
1.,0.965925826289068,1.,0.965925826289068,1.,0.965925826289068,1.,0.965925826289068,
1.,0.965925826289068,1.,0.965925826289068,1.,0.965925826289068,1.,0.965925826289068,
1.,0.965925826289068,1.,0.965925826289068,1.,0.965925826289068,1.,0.965925826289068,
1.,0.965925826289068,1.,0.965925826289068,1.,0.965925826289068,1.,0.965925826289068,
1.,0.965925826289068,1.,0.965925826289068,1.,0.965925826289068,1.,0.965925826289068,
1.,0.965925826289068,1.,0.965925826289068,1.,0.965925826289068,1.,0.965925826289068,
1.,0.965925826289068,1.,0.965925826289068,1.,0.965925826289068,1.,0.965925826289068,
1.,0.965925826289068,1.,0.965925826289068,1.,0.965925826289068,1.,0.965925826289068,
1.,0.965925826289068,1.,0.965925826289068,1.,0.965925826289068,1.,0.965925826289068,
1.,0.965925826289068,1.,0.965925826289068,1.,0.965925826289068,1.,0.965925826289068,
1.,0.965925826289068,1.,0.965925826289068,1.,0.965925826289068,1.,0.965925826289068,
1.,0.965925826289068,1.,0.965925826289068,1.,0.965925826289068,1.,0.965925826289068,
1.,0.965925826289068,1.,0.965925826289068,1.,0.965925826289068,1.,0.965925826289068,
1.,0.965925826289068,1.,0.965925826289068,1.,0.965925826289068,1.,0.965925826289068,
1.,0.965925826289068,1.,0.965925826289068,1.,0.965925826289068,1.,0.965925826289068,
1.,0.965925826289068,1.,0.965925826289068,1.,0.965925826289068,1.,0.965925826289068,
1.,0.965925826289068,1.,0.965925826289068,1.,0.965925826289068,1.,0.965925826289068,
1.,0.965925826289068,1.,0.965925826289068,1.,0.965925826289068,1.,0.965925826289068,
1.,0.965925826289068,1.,0.965925826289068,1.,0.965925826289068,1.,0.965925826289068,
1.,0.965925826289068,1.,0.965925826289068,1.,0.965925826289068,1.,0.965925826289068,
1.,0.965925826289068,1.,0.965925826289068,1.,0.965925826289068,1.,0.965925826289068,
1.,0.965925826289068,1.,0.965925826289068,1.,0.965925826289068,1.,0.965925826289068,
1.,0.965925826289068,1.,0.965925826289068,1.,0.965925826289068,1.,0.965925826289068,
1.,0.965925826289068,1.,0.965925826289068,1.,0.965925826289068,1.,0.965925826289068,
1.,0.965925826289068,1.,0.965925826289068,1.,0.965925826289068,1.,0.965925826289068,
1.,0.965925826289068,1.,0.965925826289068,1.,0.965925826289068,1.,0.965925826289068,
1.,0.965925826289068,1.,0.965925826289068,1.,0.965925826289068,1.,0.965925826289068,
1.,0.965925826289068,1.,0.965925826289068,1.,0.965925826289068,1.,0.965925826289068,
1.,0.965925826289068,1.,0.965925826289068,1.,0.965925826289068,1.,0.965925826289068,
1.,0.965925826289068,1.,0.965925826289068,1.,0.965925826289068,1.,0.965925826289068,
1.,0.965925826289068,1.,0.965925826289068,1.,0.965925826289068,1.,0.965925826289068,
1.,0.965925826289068,1.,0.965925826289068,1.,0.965925826289068,1.,0.965925826289068,
1.,0.965925826289068,1.,0.965925826289068,1.,0.965925826289068,1.,0.965925826289068,
1.,0.965925826289068,1.,0.965925826289068,1.,0.965925826289068,1.,0.965925826289068,
1.,0.965925826289068,1.,0.965925826289068,1.,0.965925826289068,1.,0.965925826289068,
1.,0.965925826289068,1.,0.965925826289068,1.,0.965925826289068,1.,0.965925826289068,
1.,0.965925826289068,1.,0.965925826289068,1.,0.965925826289068,1.,0.965925826289068,
1.,0.965925826289068,1.,0.965925826289068,1.,0.965925826289068,1.,0.965925826289068,
1.,0.965925826289068,1.,0.965925826289068,1.,0.965925826289068,1.,0.965925826289068,
1.,0.965925826289068,1.,0.965925826289068,1.,0.965925826289068,1.,0.965925826289068,
1.,0.965925826289068,1.,0.965925826289068,1.,0.965925826289068,1.,0.965925826289068,
1.,0.965925826289068,1.,0.965925826289068,1.,0.965925826289068,1.,0.965925826289068,
1.,0.965925826289068,1.,0.965925826289068,1.,0.965925826289068,1.,0.965925826289068,
1.,0.965925826289068,1.,0.965925826289068,1.,0.965925826289068,1.,0.965925826289068,
1.,0.965925826289068,1.,0.965925826289068,1.,0.965925826289068,1.,0.965925826289068,
1.,0.965925826289068,1.,0.965925826289068,1.,0.965925826289068,1.,0.965925826289068,
1.,0.965925826289068,1.,0.965925826289068,1.,0.965925826289068,1.,0.965925826289068,
1.,0.965925826289068,1.,0.965925826289068,1.,0.965925826289068,1.,0.965925826289068,
1.,0.965925826289068,1.,0.965925826289068,1.,0.965925826289068,1.,0.965925826289068,
1.,0.965925826289068,1.,0.965925826289068,1.,0.965925826289068,1.,0.965925826289068,
1.,0.965925826289068,1.,0.965925826289068,1.,0.965925826289068,1.,0.965925826289068,
1.,0.965925826289068,1.,0.965925826289068,1.,0.965925826289068,1.,0.965925826289068,
1.,0.965925826289068,1.,0.965925826289068,1.,0.965925826289068,1.,0.965925826289068,
1.,0.965925826289068,1.,0.965925826289068,1.,0.965925826289068,1.,0.965925826289068,
1.),(0.333333333333333,0.321975275429689,0.333333333333333,0.321975275429689,
0.333333333333333,0.321975275429689,0.333333333333333,0.321975275429689,
0.333333333333333,0.321975275429689,0.333333333333333,0.321975275429689,
0.333333333333333,0.321975275429689,0.333333333333333,0.321975275429689,
0.333333333333333,0.321975275429689,0.333333333333333,0.321975275429689,
0.333333333333333,0.321975275429689,0.333333333333333,0.321975275429689,
0.333333333333333,0.321975275429689,0.333333333333333,0.321975275429689,
0.333333333333333,0.321975275429689,0.333333333333333,0.321975275429689,
0.333333333333333,0.321975275429689,0.333333333333333,0.321975275429689,
0.333333333333333,0.321975275429689,0.333333333333333,0.321975275429689,
0.333333333333333,0.321975275429689,0.333333333333333,0.321975275429689,
0.333333333333333,0.321975275429689,0.333333333333333,0.321975275429689,
0.333333333333333,0.321975275429689,0.333333333333333,0.321975275429689,
0.333333333333333,0.321975275429689,0.333333333333333,0.321975275429689,
0.333333333333333,0.321975275429689,0.333333333333333,0.321975275429689,
0.333333333333333,0.321975275429689,0.333333333333333,0.321975275429689,
0.333333333333333,0.321975275429689,0.333333333333333,0.321975275429689,
0.333333333333333,0.321975275429689,0.333333333333333,0.321975275429689,
0.333333333333333,0.321975275429689,0.333333333333333,0.321975275429689,
0.333333333333333,0.321975275429689,0.333333333333333,0.321975275429689,
0.333333333333333,0.321975275429689,0.333333333333333,0.321975275429689,
0.333333333333333,0.321975275429689,0.333333333333333,0.321975275429689,
0.333333333333333,0.321975275429689,0.333333333333333,0.321975275429689,
0.333333333333333,0.321975275429689,0.333333333333333,0.321975275429689,
0.333333333333333,0.321975275429689,0.333333333333333,0.321975275429689,
0.333333333333333,0.321975275429689,0.333333333333333,0.321975275429689,
0.333333333333333,0.321975275429689,0.333333333333333,0.321975275429689,
0.333333333333333,0.321975275429689,0.333333333333333,0.321975275429689,
0.333333333333333,0.321975275429689,0.333333333333333,0.321975275429689,
0.333333333333333,0.321975275429689,0.333333333333333,0.321975275429689,
0.333333333333333,0.321975275429689,0.333333333333333,0.321975275429689,
0.333333333333333,0.321975275429689,0.333333333333333,0.321975275429689,
0.333333333333333,0.321975275429689,0.333333333333333,0.321975275429689,
0.333333333333333,0.321975275429689,0.333333333333333,0.321975275429689,
0.333333333333333,0.321975275429689,0.333333333333333,0.321975275429689,
0.333333333333333,0.321975275429689,0.333333333333333,0.321975275429689,
0.333333333333333,0.321975275429689,0.333333333333333,0.321975275429689,
0.333333333333333,0.321975275429689,0.333333333333333,0.321975275429689,
0.333333333333333,0.321975275429689,0.333333333333333,0.321975275429689,
0.333333333333333,0.321975275429689,0.333333333333333,0.321975275429689,
0.333333333333333,0.321975275429689,0.333333333333333,0.321975275429689,
0.333333333333333,0.321975275429689,0.333333333333333,0.321975275429689,
0.333333333333333,0.321975275429689,0.333333333333333,0.321975275429689,
0.333333333333333,0.321975275429689,0.333333333333333,0.321975275429689,
0.333333333333333,0.321975275429689,0.333333333333333,0.321975275429689,
0.333333333333333,0.321975275429689,0.333333333333333,0.321975275429689,
0.333333333333333,0.321975275429689,0.333333333333333,0.321975275429689,
0.333333333333333,0.321975275429689,0.333333333333333,0.321975275429689,
0.333333333333333,0.321975275429689,0.333333333333333,0.321975275429689,
0.333333333333333,0.321975275429689,0.333333333333333,0.321975275429689,
0.333333333333333,0.321975275429689,0.333333333333333,0.321975275429689,
0.333333333333333,0.321975275429689,0.333333333333333,0.321975275429689,
0.333333333333333,0.321975275429689,0.333333333333333,0.321975275429689,
0.333333333333333,0.321975275429689,0.333333333333333,0.321975275429689,
0.333333333333333,0.321975275429689,0.333333333333333,0.321975275429689,
0.333333333333333,0.321975275429689,0.333333333333333,0.321975275429689,
0.333333333333333,0.321975275429689,0.333333333333333,0.321975275429689,
0.333333333333333,0.321975275429689,0.333333333333333,0.321975275429689,
0.333333333333333,0.321975275429689,0.333333333333333,0.321975275429689,
0.333333333333333,0.321975275429689,0.333333333333333,0.321975275429689,
0.333333333333333,0.321975275429689,0.333333333333333,0.321975275429689,
0.333333333333333,0.321975275429689,0.333333333333333,0.321975275429689,
0.333333333333333,0.321975275429689,0.333333333333333,0.321975275429689,
0.333333333333333,0.321975275429689,0.333333333333333,0.321975275429689,
0.333333333333333,0.321975275429689,0.333333333333333,0.321975275429689,
0.333333333333333,0.321975275429689,0.333333333333333,0.321975275429689,
0.333333333333333,0.321975275429689,0.333333333333333,0.321975275429689,
0.333333333333333,0.321975275429689,0.333333333333333,0.321975275429689,
0.333333333333333,0.321975275429689,0.333333333333333,0.321975275429689,
0.333333333333333,0.321975275429689,0.333333333333333,0.321975275429689,
0.333333333333333,0.321975275429689,0.333333333333333,0.321975275429689,
0.333333333333333,0.321975275429689,0.333333333333333,0.321975275429689,
0.333333333333333,0.321975275429689,0.333333333333333,0.321975275429689,
0.333333333333333,0.321975275429689,0.333333333333333,0.321975275429689,
0.333333333333333,0.321975275429689,0.333333333333333,0.321975275429689,
0.333333333333333,0.321975275429689,0.333333333333333,0.321975275429689,
0.333333333333333,0.321975275429689,0.333333333333333,0.321975275429689,
0.333333333333333,0.321975275429689,0.333333333333333,0.321975275429689,
0.333333333333333,0.321975275429689,0.333333333333333,0.321975275429689,
0.333333333333333,0.321975275429689,0.333333333333333,0.321975275429689,
0.333333333333333,0.321975275429689,0.333333333333333,0.321975275429689,
0.333333333333333,0.321975275429689,0.333333333333333,0.321975275429689,
0.333333333333333,0.321975275429689,0.333333333333333,0.321975275429689,
0.333333333333333,0.321975275429689,0.333333333333333,0.321975275429689,
0.333333333333333,0.321975275429689,0.333333333333333,0.321975275429689,
0.333333333333333,0.321975275429689,0.333333333333333,0.321975275429689,
0.333333333333333,0.321975275429689,0.333333333333333,0.321975275429689,
0.333333333333333,0.321975275429689,0.333333333333333,0.321975275429689,
0.333333333333333,0.321975275429689,0.333333333333333,0.321975275429689,
0.333333333333333,0.321975275429689,0.333333333333333,0.321975275429689,
0.333333333333333,0.321975275429689,0.333333333333333,0.321975275429689,
0.333333333333333,0.321975275429689,0.333333333333333,0.321975275429689,
0.333333333333333,0.321975275429689,0.333333333333333,0.321975275429689,
0.333333333333333,0.321975275429689,0.333333333333333,0.321975275429689,
0.333333333333333,0.321975275429689,0.333333333333333,0.321975275429689,
0.333333333333333,0.321975275429689,0.333333333333333,0.321975275429689,
0.333333333333333,0.321975275429689,0.333333333333333,0.321975275429689,
0.333333333333333,0.321975275429689,0.333333333333333,0.321975275429689,
0.333333333333333,0.321975275429689,0.333333333333333,0.321975275429689,
0.333333333333333,0.321975275429689,0.333333333333333,0.321975275429689,
0.333333333333333,0.321975275429689,0.333333333333333,0.321975275429689,
0.333333333333333,0.321975275429689,0.333333333333333,0.321975275429689,
0.333333333333333,0.321975275429689,0.333333333333333,0.321975275429689,
0.333333333333333,0.321975275429689,0.333333333333333,0.321975275429689,
0.333333333333333,0.321975275429689,0.333333333333333,0.321975275429689,
0.333333333333333,0.321975275429689,0.333333333333333,0.321975275429689,
0.333333333333333,0.321975275429689,0.333333333333333,0.321975275429689,
0.333333333333333,0.321975275429689,0.333333333333333,0.321975275429689,
0.333333333333333,0.321975275429689,0.333333333333333,0.321975275429689,
0.333333333333333,0.321975275429689,0.333333333333333,0.321975275429689,
0.333333333333333,0.321975275429689,0.333333333333333,0.321975275429689,
0.333333333333333,0.321975275429689,0.333333333333333,0.321975275429689,
0.333333333333333,0.321975275429689,0.333333333333333,0.321975275429689,
0.333333333333333,0.321975275429689,0.333333333333333,0.321975275429689,
0.333333333333333),(0.333333333333333,0.321975275429689,0.333333333333333,
0.321975275429689,0.333333333333333,0.321975275429689,0.333333333333333,
0.321975275429689,0.333333333333333,0.321975275429689,0.333333333333333,
0.321975275429689,0.333333333333333,0.321975275429689,0.333333333333333,
0.321975275429689,0.333333333333333,0.321975275429689,0.333333333333333,
0.321975275429689,0.333333333333333,0.321975275429689,0.333333333333333,
0.321975275429689,0.333333333333333,0.321975275429689,0.333333333333333,
0.321975275429689,0.333333333333333,0.321975275429689,0.333333333333333,
0.321975275429689,0.333333333333333,0.321975275429689,0.333333333333333,
0.321975275429689,0.333333333333333,0.321975275429689,0.333333333333333,
0.321975275429689,0.333333333333333,0.321975275429689,0.333333333333333,
0.321975275429689,0.333333333333333,0.321975275429689,0.333333333333333,
0.321975275429689,0.333333333333333,0.321975275429689,0.333333333333333,
0.321975275429689,0.333333333333333,0.321975275429689,0.333333333333333,
0.321975275429689,0.333333333333333,0.321975275429689,0.333333333333333,
0.321975275429689,0.333333333333333,0.321975275429689,0.333333333333333,
0.321975275429689,0.333333333333333,0.321975275429689,0.333333333333333,
0.321975275429689,0.333333333333333,0.321975275429689,0.333333333333333,
0.321975275429689,0.333333333333333,0.321975275429689,0.333333333333333,
0.321975275429689,0.333333333333333,0.321975275429689,0.333333333333333,
0.321975275429689,0.333333333333333,0.321975275429689,0.333333333333333,
0.321975275429689,0.333333333333333,0.321975275429689,0.333333333333333,
0.321975275429689,0.333333333333333,0.321975275429689,0.333333333333333,
0.321975275429689,0.333333333333333,0.321975275429689,0.333333333333333,
0.321975275429689,0.333333333333333,0.321975275429689,0.333333333333333,
0.321975275429689,0.333333333333333,0.321975275429689,0.333333333333333,
0.321975275429689,0.333333333333333,0.321975275429689,0.333333333333333,
0.321975275429689,0.333333333333333,0.321975275429689,0.333333333333333,
0.321975275429689,0.333333333333333,0.321975275429689,0.333333333333333,
0.321975275429689,0.333333333333333,0.321975275429689,0.333333333333333,
0.321975275429689,0.333333333333333,0.321975275429689,0.333333333333333,
0.321975275429689,0.333333333333333,0.321975275429689,0.333333333333333,
0.321975275429689,0.333333333333333,0.321975275429689,0.333333333333333,
0.321975275429689,0.333333333333333,0.321975275429689,0.333333333333333,
0.321975275429689,0.333333333333333,0.321975275429689,0.333333333333333,
0.321975275429689,0.333333333333333,0.321975275429689,0.333333333333333,
0.321975275429689,0.333333333333333,0.321975275429689,0.333333333333333,
0.321975275429689,0.333333333333333,0.321975275429689,0.333333333333333,
0.321975275429689,0.333333333333333,0.321975275429689,0.333333333333333,
0.321975275429689,0.333333333333333,0.321975275429689,0.333333333333333,
0.321975275429689,0.333333333333333,0.321975275429689,0.333333333333333,
0.321975275429689,0.333333333333333,0.321975275429689,0.333333333333333,
0.321975275429689,0.333333333333333,0.321975275429689,0.333333333333333,
0.321975275429689,0.333333333333333,0.321975275429689,0.333333333333333,
0.321975275429689,0.333333333333333,0.321975275429689,0.333333333333333,
0.321975275429689,0.333333333333333,0.321975275429689,0.333333333333333,
0.321975275429689,0.333333333333333,0.321975275429689,0.333333333333333,
0.321975275429689,0.333333333333333,0.321975275429689,0.333333333333333,
0.321975275429689,0.333333333333333,0.321975275429689,0.333333333333333,
0.321975275429689,0.333333333333333,0.321975275429689,0.333333333333333,
0.321975275429689,0.333333333333333,0.321975275429689,0.333333333333333,
0.321975275429689,0.333333333333333,0.321975275429689,0.333333333333333,
0.321975275429689,0.333333333333333,0.321975275429689,0.333333333333333,
0.321975275429689,0.333333333333333,0.321975275429689,0.333333333333333,
0.321975275429689,0.333333333333333,0.321975275429689,0.333333333333333,
0.321975275429689,0.333333333333333,0.321975275429689,0.333333333333333,
0.321975275429689,0.333333333333333,0.321975275429689,0.333333333333333,
0.321975275429689,0.333333333333333,0.321975275429689,0.333333333333333,
0.321975275429689,0.333333333333333,0.321975275429689,0.333333333333333,
0.321975275429689,0.333333333333333,0.321975275429689,0.333333333333333,
0.321975275429689,0.333333333333333,0.321975275429689,0.333333333333333,
0.321975275429689,0.333333333333333,0.321975275429689,0.333333333333333,
0.321975275429689,0.333333333333333,0.321975275429689,0.333333333333333,
0.321975275429689,0.333333333333333,0.321975275429689,0.333333333333333,
0.321975275429689,0.333333333333333,0.321975275429689,0.333333333333333,
0.321975275429689,0.333333333333333,0.321975275429689,0.333333333333333,
0.321975275429689,0.333333333333333,0.321975275429689,0.333333333333333,
0.321975275429689,0.333333333333333,0.321975275429689,0.333333333333333,
0.321975275429689,0.333333333333333,0.321975275429689,0.333333333333333,
0.321975275429689,0.333333333333333,0.321975275429689,0.333333333333333,
0.321975275429689,0.333333333333333,0.321975275429689,0.333333333333333,
0.321975275429689,0.333333333333333,0.321975275429689,0.333333333333333,
0.321975275429689,0.333333333333333,0.321975275429689,0.333333333333333,
0.321975275429689,0.333333333333333,0.321975275429689,0.333333333333333,
0.321975275429689,0.333333333333333,0.321975275429689,0.333333333333333,
0.321975275429689,0.333333333333333,0.321975275429689,0.333333333333333,
0.321975275429689,0.333333333333333,0.321975275429689,0.333333333333333,
0.321975275429689,0.333333333333333,0.321975275429689,0.333333333333333,
0.321975275429689,0.333333333333333,0.321975275429689,0.333333333333333,
0.321975275429689,0.333333333333333,0.321975275429689,0.333333333333333,
0.321975275429689,0.333333333333333,0.321975275429689,0.333333333333333,
0.321975275429689,0.333333333333333,0.321975275429689,0.333333333333333,
0.321975275429689,0.333333333333333,0.321975275429689,0.333333333333333,
0.321975275429689,0.333333333333333,0.321975275429689,0.333333333333333,
0.321975275429689,0.333333333333333,0.321975275429689,0.333333333333333,
0.321975275429689,0.333333333333333,0.321975275429689,0.333333333333333,
0.321975275429689,0.333333333333333,0.321975275429689,0.333333333333333,
0.321975275429689,0.333333333333333,0.321975275429689,0.333333333333333,
0.321975275429689,0.333333333333333,0.321975275429689,0.333333333333333,
0.321975275429689,0.333333333333333,0.321975275429689,0.333333333333333,
0.321975275429689,0.333333333333333,0.321975275429689,0.333333333333333,
0.321975275429689,0.333333333333333,0.321975275429689,0.333333333333333,
0.321975275429689,0.333333333333333,0.321975275429689,0.333333333333333,
0.321975275429689,0.333333333333333,0.321975275429689,0.333333333333333,
0.321975275429689,0.333333333333333,0.321975275429689,0.333333333333333,
0.321975275429689,0.333333333333333,0.321975275429689,0.333333333333333,
0.321975275429689,0.333333333333333,0.321975275429689,0.333333333333333,
0.321975275429689,0.333333333333333,0.321975275429689,0.333333333333333,
0.321975275429689,0.333333333333333,0.321975275429689,0.333333333333333,
0.321975275429689,0.333333333333333,0.321975275429689,0.333333333333333,
0.321975275429689,0.333333333333333,0.321975275429689,0.333333333333333,
0.321975275429689,0.333333333333333,0.321975275429689,0.333333333333333,
0.321975275429689,0.333333333333333,0.321975275429689,0.333333333333333,
0.321975275429689,0.333333333333333,0.321975275429689,0.333333333333333,
0.321975275429689,0.333333333333333,0.321975275429689,0.333333333333333,
0.321975275429689,0.333333333333333,0.321975275429689,0.333333333333333,
0.321975275429689,0.333333333333333,0.321975275429689,0.333333333333333,
0.321975275429689,0.333333333333333,0.321975275429689,0.333333333333333,
0.321975275429689,0.333333333333333,0.321975275429689,0.333333333333333,
0.321975275429689,0.333333333333333,0.321975275429689,0.333333333333333,
0.321975275429689,0.333333333333333,0.321975275429689,0.333333333333333,
0.321975275429689,0.333333333333333,0.321975275429689,0.333333333333333,
0.321975275429689,0.333333333333333,0.321975275429689,0.333333333333333,
0.321975275429689,0.333333333333333,0.321975275429689,0.333333333333333,
0.321975275429689,0.333333333333333),(1.,0.965925826289068,1.,0.965925826289068,
1.,0.965925826289068,1.,0.965925826289068,1.,0.965925826289068,1.,0.965925826289068,
1.,0.965925826289068,1.,0.965925826289068,1.,0.965925826289068,1.,0.965925826289068,
1.,0.965925826289068,1.,0.965925826289068,1.,0.965925826289068,1.,0.965925826289068,
1.,0.965925826289068,1.,0.965925826289068,1.,0.965925826289068,1.,0.965925826289068,
1.,0.965925826289068,1.,0.965925826289068,1.,0.965925826289068,1.,0.965925826289068,
1.,0.965925826289068,1.,0.965925826289068,1.,0.965925826289068,1.,0.965925826289068,
1.,0.965925826289068,1.,0.965925826289068,1.,0.965925826289068,1.,0.965925826289068,
1.,0.965925826289068,1.,0.965925826289068,1.,0.965925826289068,1.,0.965925826289068,
1.,0.965925826289068,1.,0.965925826289068,1.,0.965925826289068,1.,0.965925826289068,
1.,0.965925826289068,1.,0.965925826289068,1.,0.965925826289068,1.,0.965925826289068,
1.,0.965925826289068,1.,0.965925826289068,1.,0.965925826289068,1.,0.965925826289068,
1.,0.965925826289068,1.,0.965925826289068,1.,0.965925826289068,1.,0.965925826289068,
1.,0.965925826289068,1.,0.965925826289068,1.,0.965925826289068,1.,0.965925826289068,
1.,0.965925826289068,1.,0.965925826289068,1.,0.965925826289068,1.,0.965925826289068,
1.,0.965925826289068,1.,0.965925826289068,1.,0.965925826289068,1.,0.965925826289068,
1.,0.965925826289068,1.,0.965925826289068,1.,0.965925826289068,1.,0.965925826289068,
1.,0.965925826289068,1.,0.965925826289068,1.,0.965925826289068,1.,0.965925826289068,
1.,0.965925826289068,1.,0.965925826289068,1.,0.965925826289068,1.,0.965925826289068,
1.,0.965925826289068,1.,0.965925826289068,1.,0.965925826289068,1.,0.965925826289068,
1.,0.965925826289068,1.,0.965925826289068,1.,0.965925826289068,1.,0.965925826289068,
1.,0.965925826289068,1.,0.965925826289068,1.,0.965925826289068,1.,0.965925826289068,
1.,0.965925826289068,1.,0.965925826289068,1.,0.965925826289068,1.,0.965925826289068,
1.,0.965925826289068,1.,0.965925826289068,1.,0.965925826289068,1.,0.965925826289068,
1.,0.965925826289068,1.,0.965925826289068,1.,0.965925826289068,1.,0.965925826289068,
1.,0.965925826289068,1.,0.965925826289068,1.,0.965925826289068,1.,0.965925826289068,
1.,0.965925826289068,1.,0.965925826289068,1.,0.965925826289068,1.,0.965925826289068,
1.,0.965925826289068,1.,0.965925826289068,1.,0.965925826289068,1.,0.965925826289068,
1.,0.965925826289068,1.,0.965925826289068,1.,0.965925826289068,1.,0.965925826289068,
1.,0.965925826289068,1.,0.965925826289068,1.,0.965925826289068,1.,0.965925826289068,
1.,0.965925826289068,1.,0.965925826289068,1.,0.965925826289068,1.,0.965925826289068,
1.,0.965925826289068,1.,0.965925826289068,1.,0.965925826289068,1.,0.965925826289068,
1.,0.965925826289068,1.,0.965925826289068,1.,0.965925826289068,1.,0.965925826289068,
1.,0.965925826289068,1.,0.965925826289068,1.,0.965925826289068,1.,0.965925826289068,
1.,0.965925826289068,1.,0.965925826289068,1.,0.965925826289068,1.,0.965925826289068,
1.,0.965925826289068,1.,0.965925826289068,1.,0.965925826289068,1.,0.965925826289068,
1.,0.965925826289068,1.,0.965925826289068,1.,0.965925826289068,1.,0.965925826289068,
1.,0.965925826289068,1.,0.965925826289068,1.,0.965925826289068,1.,0.965925826289068,
1.,0.965925826289068,1.,0.965925826289068,1.,0.965925826289068,1.,0.965925826289068,
1.,0.965925826289068,1.,0.965925826289068,1.,0.965925826289068,1.,0.965925826289068,
1.,0.965925826289068,1.,0.965925826289068,1.,0.965925826289068,1.,0.965925826289068,
1.,0.965925826289068,1.,0.965925826289068,1.,0.965925826289068,1.,0.965925826289068,
1.,0.965925826289068,1.,0.965925826289068,1.,0.965925826289068,1.,0.965925826289068,
1.,0.965925826289068,1.,0.965925826289068,1.,0.965925826289068,1.,0.965925826289068,
1.,0.965925826289068,1.,0.965925826289068,1.,0.965925826289068,1.,0.965925826289068,
1.,0.965925826289068,1.,0.965925826289068,1.,0.965925826289068,1.,0.965925826289068,
1.,0.965925826289068,1.,0.965925826289068,1.,0.965925826289068,1.,0.965925826289068,
1.,0.965925826289068,1.,0.965925826289068,1.,0.965925826289068,1.,0.965925826289068,
1.,0.965925826289068,1.,0.965925826289068,1.,0.965925826289068,1.,0.965925826289068,
1.,0.965925826289068,1.,0.965925826289068,1.,0.965925826289068,1.,0.965925826289068,
1.,0.965925826289068,1.,0.965925826289068,1.,0.965925826289068,1.,0.965925826289068,
1.,0.965925826289068,1.,0.965925826289068,1.,0.965925826289068,1.,0.965925826289068,
1.,0.965925826289068,1.,0.965925826289068,1.,0.965925826289068,1.,0.965925826289068,
1.,0.965925826289068,1.,0.965925826289068,1.,0.965925826289068,1.,0.965925826289068,
1.,0.965925826289068,1.,0.965925826289068,1.,0.965925826289068,1.,0.965925826289068,
1.,0.965925826289068,1.,0.965925826289068,1.,0.965925826289068,1.,0.965925826289068,
1.,0.965925826289068,1.,0.965925826289068,1.,0.965925826289068,1.,0.965925826289068,
1.,0.965925826289068,1.,0.965925826289068,1.)))
REPRESENTATION_ITEM('')
SURFACE()
);
#460=(
BOUNDED_SURFACE()
B_SPLINE_SURFACE(3,2,((#30126,#30127,#30128),(#30129,#30130,#30131),(#30132,
#30133,#30134),(#30135,#30136,#30137),(#30138,#30139,#30140),(#30141,#30142,
#30143),(#30144,#30145,#30146),(#30147,#30148,#30149),(#30150,#30151,#30152),
(#30153,#30154,#30155),(#30156,#30157,#30158),(#30159,#30160,#30161),(#30162,
#30163,#30164),(#30165,#30166,#30167),(#30168,#30169,#30170),(#30171,#30172,
#30173),(#30174,#30175,#30176),(#30177,#30178,#30179),(#30180,#30181,#30182),
(#30183,#30184,#30185),(#30186,#30187,#30188),(#30189,#30190,#30191)),
 .UNSPECIFIED.,.F.,.F.,.F.)
B_SPLINE_SURFACE_WITH_KNOTS((4,2,2,2,2,2,2,2,2,2,4),(3,3),(0.00618007368741724,
0.00707169626481771,0.00796331884221818,0.00885494141961865,0.00930075270831889,
0.00974656399701912,0.0101923752857194,0.0106381865744196,0.0115298091518201,
0.0124214317292205,0.013313054306621),(0.,1.),.UNSPECIFIED.)
GEOMETRIC_REPRESENTATION_ITEM()
RATIONAL_B_SPLINE_SURFACE(((1.,0.858045858703177,1.),(1.,0.866904822687482,
1.),(1.,0.875299209011426,1.),(1.,0.890836089594423,1.),(1.,0.898040712548752,
1.),(1.,0.910117038219606,1.),(1.,0.915056450314983,1.),(1.,0.920263585253285,
1.),(1.,0.921616129399948,1.),(1.,0.923410100119622,1.),(1.,0.923869223474666,
1.),(1.,0.923889498575711,1.),(1.,0.92344256786583,1.),(1.,0.921656854892037,
1.),(1.,0.920333354099966,1.),(1.,0.9152042866524,1.),(1.,0.910157237148985,
1.),(1.,0.898027307649231,1.),(1.,0.890964714100696,1.),(1.,0.875368043550207,
1.),(1.,0.86682243570435,1.),(1.,0.85805265757134,1.)))
REPRESENTATION_ITEM('')
SURFACE()
);
#461=(
BOUNDED_SURFACE()
B_SPLINE_SURFACE(3,2,((#30228,#30229,#30230),(#30231,#30232,#30233),(#30234,
#30235,#30236),(#30237,#30238,#30239),(#30240,#30241,#30242),(#30243,#30244,
#30245),(#30246,#30247,#30248),(#30249,#30250,#30251),(#30252,#30253,#30254),
(#30255,#30256,#30257),(#30258,#30259,#30260),(#30261,#30262,#30263),(#30264,
#30265,#30266),(#30267,#30268,#30269),(#30270,#30271,#30272),(#30273,#30274,
#30275),(#30276,#30277,#30278),(#30279,#30280,#30281),(#30282,#30283,#30284),
(#30285,#30286,#30287),(#30288,#30289,#30290),(#30291,#30292,#30293)),
 .UNSPECIFIED.,.F.,.F.,.F.)
B_SPLINE_SURFACE_WITH_KNOTS((4,2,2,2,2,2,2,2,2,2,4),(3,3),(0.00463173145868099,
0.0055550496708318,0.00644833560515975,0.00689497857232373,0.0073416215394877,
0.00823490747381566,0.00868155044097963,0.00912819340814361,0.0100214793424716,
0.0109147652767995,0.011838209828059),(-9.16721149006242E-5,1.00007252857048),
 .UNSPECIFIED.)
GEOMETRIC_REPRESENTATION_ITEM()
RATIONAL_B_SPLINE_SURFACE(((1.00002619145898,0.857135625077539,1.00002072159804),
(1.00002451884082,0.866259116387597,1.0000193982918),(1.00002289154787,
0.875135376031697,1.00001811084498),(1.00001998551899,0.890986650264669,
1.00001581171524),(1.00001868879555,0.898059779870719,1.00001478580134),
(1.00001701652053,0.90718139945745,1.00001346276657),(1.00001650323434,
0.909981178978598,1.00001305667579),(1.00001560966983,0.914855231051331,
1.00001234972454),(1.00001522637194,0.916945974201243,1.00001204647512),
(1.00001428784851,0.922065259968938,1.00001130395424),(1.00001395123475,
0.923901359098063,1.00001103763936),(1.0000139608147,0.923849104111275,
1.00001104521863),(1.00001404571456,0.923386007914237,1.00001111238788),
(1.00001437612857,0.921583726099594,1.00001137379776),(1.00001462510049,
0.920225679629222,1.00001157077404),(1.00001558266984,0.915002505660967,
1.00001232836327),(1.00001648988299,0.910054005470624,1.00001304611276),
(1.00001870584049,0.897966806240844,1.00001479928659),(1.000020028908,0.890749979859378,
1.00001584604283),(1.00002292411145,0.87495775415132,1.00001813660794),
(1.00002451487478,0.866280749609431,1.00001939515403),(1.00002619181141,
0.857133702726523,1.00002072187687)))
REPRESENTATION_ITEM('')
SURFACE()
);
#462=(
BOUNDED_SURFACE()
B_SPLINE_SURFACE(3,2,((#30330,#30331,#30332),(#30333,#30334,#30335),(#30336,
#30337,#30338),(#30339,#30340,#30341),(#30342,#30343,#30344),(#30345,#30346,
#30347),(#30348,#30349,#30350),(#30351,#30352,#30353),(#30354,#30355,#30356),
(#30357,#30358,#30359),(#30360,#30361,#30362),(#30363,#30364,#30365),(#30366,
#30367,#30368),(#30369,#30370,#30371),(#30372,#30373,#30374),(#30375,#30376,
#30377),(#30378,#30379,#30380),(#30381,#30382,#30383)),.UNSPECIFIED.,.F.,
 .F.,.F.)
B_SPLINE_SURFACE_WITH_KNOTS((4,2,2,2,2,2,2,2,4),(3,3),(0.00330583080240976,
0.0050987612729038,0.00599522650815083,0.00689169174339785,0.00733992436102137,
0.00778815697864488,0.0086846222138919,0.00958108744913893,0.010477552684386),
(0.,1.),.UNSPECIFIED.)
GEOMETRIC_REPRESENTATION_ITEM()
RATIONAL_B_SPLINE_SURFACE(((1.,0.858051573205352,1.),(1.,0.875590740245255,
1.),(1.,0.891984535276897,1.),(1.,0.910123535489779,1.),(1.,0.915171726878822,
1.),(1.,0.922080092984598,1.),(1.,0.923887406776032,1.),(1.,0.923875556180348,
1.),(1.,0.923415662237232,1.),(1.,0.921609909018457,1.),(1.,0.920278779497026,
1.),(1.,0.91513274798944,1.),(1.,0.910082531829078,1.),(1.,0.897961000925969,
1.),(1.,0.890907866965291,1.),(1.,0.875336477322621,1.),(1.,0.866807510696487,
1.),(1.,0.858055143785041,1.)))
REPRESENTATION_ITEM('')
SURFACE()
);
#463=(
BOUNDED_SURFACE()
B_SPLINE_SURFACE(3,2,((#30435,#30436,#30437),(#30438,#30439,#30440),(#30441,
#30442,#30443),(#30444,#30445,#30446),(#30447,#30448,#30449),(#30450,#30451,
#30452),(#30453,#30454,#30455),(#30456,#30457,#30458),(#30459,#30460,#30461),
(#30462,#30463,#30464),(#30465,#30466,#30467),(#30468,#30469,#30470),(#30471,
#30472,#30473),(#30474,#30475,#30476),(#30477,#30478,#30479),(#30480,#30481,
#30482),(#30483,#30484,#30485),(#30486,#30487,#30488),(#30489,#30490,#30491),
(#30492,#30493,#30494),(#30495,#30496,#30497),(#30498,#30499,#30500)),
 .UNSPECIFIED.,.F.,.F.,.F.)
B_SPLINE_SURFACE_WITH_KNOTS((4,2,2,2,2,2,2,2,2,2,4),(3,3),(0.00463173145912357,
0.0055550496708318,0.00644833560515975,0.00689497857232373,0.0073416215394877,
0.00823490747381566,0.00868155044097963,0.00912819340814361,0.0100214793424716,
0.0109147652767995,0.0118382098276163),(-9.16721145407206E-5,1.00007252857004),
 .UNSPECIFIED.)
GEOMETRIC_REPRESENTATION_ITEM()
RATIONAL_B_SPLINE_SURFACE(((1.00002619145888,0.857135625090785,1.00002072159791),
(1.00002451884072,0.866259116396099,1.00001939829168),(1.00002289154778,
0.875135376035797,1.00001811084487),(1.00001998551891,0.890986650264622,
1.00001581171514),(1.00001868879548,0.898059779870952,1.00001478580125),
(1.00001701652046,0.907181399457448,1.00001346276649),(1.00001650323428,
0.909981178978704,1.00001305667571),(1.00001560966977,0.914855231051366,
1.00001234972447),(1.00001522637188,0.916945974201386,1.00001204647505),
(1.00001428784846,0.922065259968851,1.00001130395417),(1.00001395123469,
0.923901359098042,1.0000110376393),(1.00001396081465,0.923849104111378,
1.00001104521856),(1.00001404571451,0.923386007914241,1.00001111238781),
(1.00001437612851,0.921583726099716,1.00001137379769),(1.00001462510043,
0.920225679629301,1.00001157077397),(1.00001558266978,0.915002505661001,
1.00001232836319),(1.00001648988293,0.910054005470596,1.00001304611268),
(1.00001870584042,0.897966806241025,1.0000147992865),(1.00002002890792,
0.890749979859465,1.00001584604273),(1.00002292411136,0.874957754155268,
1.00001813660783),(1.00002451487468,0.866280749617856,1.00001939515391),
(1.0000261918113,0.857133702739791,1.00002072187674)))
REPRESENTATION_ITEM('')
SURFACE()
);
#464=(
BOUNDED_SURFACE()
B_SPLINE_SURFACE(3,2,((#30537,#30538,#30539),(#30540,#30541,#30542),(#30543,
#30544,#30545),(#30546,#30547,#30548),(#30549,#30550,#30551),(#30552,#30553,
#30554),(#30555,#30556,#30557),(#30558,#30559,#30560),(#30561,#30562,#30563),
(#30564,#30565,#30566),(#30567,#30568,#30569),(#30570,#30571,#30572),(#30573,
#30574,#30575),(#30576,#30577,#30578),(#30579,#30580,#30581),(#30582,#30583,
#30584),(#30585,#30586,#30587),(#30588,#30589,#30590)),.UNSPECIFIED.,.F.,
 .F.,.F.)
B_SPLINE_SURFACE_WITH_KNOTS((4,2,2,2,2,2,2,2,4),(3,3),(0.0033058308024097,
0.00509876127290375,0.00599522650815077,0.00689169174339779,0.0073399243610213,
0.00778815697864482,0.00868462221389184,0.00958108744913886,0.0104775526843859),
(0.,1.),.UNSPECIFIED.)
GEOMETRIC_REPRESENTATION_ITEM()
RATIONAL_B_SPLINE_SURFACE(((1.,0.858051573205352,1.),(1.,0.875590740245157,
1.),(1.,0.891984535277027,1.),(1.,0.91012353548971,1.),(1.,0.915171726878704,
1.),(1.,0.922080092984716,1.),(1.,0.923887406776032,1.),(1.,0.923875556180348,
1.),(1.,0.923415662237307,1.),(1.,0.921609909018382,1.),(1.,0.920278779497094,
1.),(1.,0.915132747989309,1.),(1.,0.910082531829295,1.),(1.,0.897961000925752,
1.),(1.,0.890907866965658,1.),(1.,0.875336477322253,1.),(1.,0.866807510696761,
1.),(1.,0.858055143785041,1.)))
REPRESENTATION_ITEM('')
SURFACE()
);
#465=(
BOUNDED_SURFACE()
B_SPLINE_SURFACE(3,2,((#30642,#30643,#30644),(#30645,#30646,#30647),(#30648,
#30649,#30650),(#30651,#30652,#30653),(#30654,#30655,#30656),(#30657,#30658,
#30659),(#30660,#30661,#30662),(#30663,#30664,#30665),(#30666,#30667,#30668),
(#30669,#30670,#30671),(#30672,#30673,#30674),(#30675,#30676,#30677),(#30678,
#30679,#30680),(#30681,#30682,#30683),(#30684,#30685,#30686),(#30687,#30688,
#30689),(#30690,#30691,#30692),(#30693,#30694,#30695),(#30696,#30697,#30698),
(#30699,#30700,#30701),(#30702,#30703,#30704),(#30705,#30706,#30707)),
 .UNSPECIFIED.,.F.,.F.,.F.)
B_SPLINE_SURFACE_WITH_KNOTS((4,2,2,2,2,2,2,2,2,2,4),(3,3),(0.00618007368741721,
0.00707169626481767,0.00796331884221814,0.00885494141961861,0.00930075270831885,
0.00974656399701908,0.0101923752857193,0.0106381865744195,0.01152980915182,
0.0124214317292205,0.013313054306621),(0.,1.),.UNSPECIFIED.)
GEOMETRIC_REPRESENTATION_ITEM()
RATIONAL_B_SPLINE_SURFACE(((1.,0.858045858703177,1.),(1.,0.86690482268742,
1.),(1.,0.875299209011509,1.),(1.,0.890836089594339,1.),(1.,0.898040712548885,
1.),(1.,0.910117038219473,1.),(1.,0.915056450314664,1.),(1.,0.920263585253445,
1.),(1.,0.921616129400065,1.),(1.,0.923410100119505,1.),(1.,0.923869223474666,
1.),(1.,0.923889498575711,1.),(1.,0.923442567865973,1.),(1.,0.921656854891893,
1.),(1.,0.92033335410005,1.),(1.,0.915204286652234,1.),(1.,0.910157237148985,
1.),(1.,0.898027307649231,1.),(1.,0.890964714100597,1.),(1.,0.875368043550308,
1.),(1.,0.866822435704274,1.),(1.,0.85805265757134,1.)))
REPRESENTATION_ITEM('')
SURFACE()
);
#466=(
BOUNDED_SURFACE()
B_SPLINE_SURFACE(3,2,((#30744,#30745,#30746),(#30747,#30748,#30749),(#30750,
#30751,#30752),(#30753,#30754,#30755),(#30756,#30757,#30758),(#30759,#30760,
#30761),(#30762,#30763,#30764),(#30765,#30766,#30767),(#30768,#30769,#30770),
(#30771,#30772,#30773),(#30774,#30775,#30776),(#30777,#30778,#30779),(#30780,
#30781,#30782),(#30783,#30784,#30785),(#30786,#30787,#30788),(#30789,#30790,
#30791),(#30792,#30793,#30794),(#30795,#30796,#30797),(#30798,#30799,#30800),
(#30801,#30802,#30803),(#30804,#30805,#30806),(#30807,#30808,#30809)),
 .UNSPECIFIED.,.F.,.F.,.F.)
B_SPLINE_SURFACE_WITH_KNOTS((4,2,2,2,2,2,2,2,2,2,4),(3,3),(0.00463173145890188,
0.0055550496708318,0.00644833560515975,0.00689497857232372,0.0073416215394877,
0.00823490747381565,0.00868155044097963,0.00912819340814361,0.0100214793424716,
0.0109147652767995,0.0118382098278381),(-9.16721146127048E-5,1.00007252857026),
 .UNSPECIFIED.)
GEOMETRIC_REPRESENTATION_ITEM()
RATIONAL_B_SPLINE_SURFACE(((1.0000261914589,0.857135625084157,1.00002072159798),
(1.00002451884074,0.86625911639194,1.00001939829174),(1.0000228915478,0.875135376033654,
1.00001811084493),(1.00001998551893,0.890986650264758,1.00001581171519),
(1.00001868879549,0.89805977987109,1.00001478580129),(1.00001701652048,
0.907181399457338,1.00001346276653),(1.00001650323429,0.909981178978669,
1.00001305667575),(1.00001560966978,0.914855231051349,1.00001234972451),
(1.0000152263719,0.916945974201319,1.00001204647509),(1.00001428784847,
0.922065259968911,1.0000113039542),(1.00001395123471,0.923901359098102,
1.00001103763933),(1.00001396081466,0.923849104111314,1.00001104521859),
(1.00001404571452,0.923386007914268,1.00001111238785),(1.00001437612852,
0.921583726099643,1.00001137379773),(1.00001462510045,0.920225679629262,
1.00001157077401),(1.00001558266979,0.915002505661011,1.00001232836323),
(1.00001648988294,0.910054005470637,1.00001304611272),(1.00001870584043,
0.897966806240929,1.00001479928655),(1.00002002890793,0.890749979859433,
1.00001584604278),(1.00002292411138,0.874957754153303,1.00001813660789),
(1.0000245148747,0.866280749613647,1.00001939515397),(1.00002619181133,
0.857133702733158,1.0000207218768)))
REPRESENTATION_ITEM('')
SURFACE()
);
#467=(
BOUNDED_SURFACE()
B_SPLINE_SURFACE(3,2,((#30846,#30847,#30848),(#30849,#30850,#30851),(#30852,
#30853,#30854),(#30855,#30856,#30857),(#30858,#30859,#30860),(#30861,#30862,
#30863),(#30864,#30865,#30866),(#30867,#30868,#30869),(#30870,#30871,#30872),
(#30873,#30874,#30875),(#30876,#30877,#30878),(#30879,#30880,#30881),(#30882,
#30883,#30884),(#30885,#30886,#30887),(#30888,#30889,#30890),(#30891,#30892,
#30893),(#30894,#30895,#30896),(#30897,#30898,#30899)),.UNSPECIFIED.,.F.,
 .F.,.F.)
B_SPLINE_SURFACE_WITH_KNOTS((4,2,2,2,2,2,2,2,4),(3,3),(0.00330583080240973,
0.00509876127290377,0.0059952265081508,0.00689169174339782,0.00733992436102133,
0.00778815697864484,0.00868462221389187,0.00958108744913889,0.0104775526843859),
(0.,1.),.UNSPECIFIED.)
GEOMETRIC_REPRESENTATION_ITEM()
RATIONAL_B_SPLINE_SURFACE(((1.,0.858051573205352,1.),(1.,0.875590740245257,
1.),(1.,0.891984535276895,1.),(1.,0.910123535489777,1.),(1.,0.915171726878671,
1.),(1.,0.92208009298475,1.),(1.,0.923887406775965,1.),(1.,0.923875556180381,
1.),(1.,0.923415662237265,1.),(1.,0.921609909018423,1.),(1.,0.920278779497103,
1.),(1.,0.915132747989292,1.),(1.,0.910082531829227,1.),(1.,0.897961000925819,
1.),(1.,0.890907866965258,1.),(1.,0.875336477322655,1.),(1.,0.86680751069646,
1.),(1.,0.858055143785041,1.)))
REPRESENTATION_ITEM('')
SURFACE()
);
#468=(
BOUNDED_SURFACE()
B_SPLINE_SURFACE(3,2,((#30951,#30952,#30953),(#30954,#30955,#30956),(#30957,
#30958,#30959),(#30960,#30961,#30962),(#30963,#30964,#30965),(#30966,#30967,
#30968),(#30969,#30970,#30971),(#30972,#30973,#30974),(#30975,#30976,#30977),
(#30978,#30979,#30980),(#30981,#30982,#30983),(#30984,#30985,#30986),(#30987,
#30988,#30989),(#30990,#30991,#30992),(#30993,#30994,#30995),(#30996,#30997,
#30998),(#30999,#31000,#31001),(#31002,#31003,#31004),(#31005,#31006,#31007),
(#31008,#31009,#31010),(#31011,#31012,#31013),(#31014,#31015,#31016)),
 .UNSPECIFIED.,.F.,.F.,.F.)
B_SPLINE_SURFACE_WITH_KNOTS((4,2,2,2,2,2,2,2,2,2,4),(3,3),(0.00463173145913793,
0.0055550496708318,0.00644833560515975,0.00689497857232373,0.0073416215394877,
0.00823490747381566,0.00868155044097963,0.00912819340814361,0.0100214793424716,
0.0109147652767995,0.011838209827602),(-9.1672114921884E-5,1.00007252857003),
 .UNSPECIFIED.)
GEOMETRIC_REPRESENTATION_ITEM()
RATIONAL_B_SPLINE_SURFACE(((1.00002619145899,0.857135625091139,1.00002072159791),
(1.00002451884082,0.866259116396527,1.00001939829167),(1.00002289154787,
0.875135376035635,1.00001811084487),(1.000019985519,0.890986650264817,1.00001581171514),
(1.00001868879555,0.898059779870914,1.00001478580124),(1.00001701652053,
0.907181399457414,1.00001346276649),(1.00001650323435,0.909981178978654,
1.00001305667571),(1.00001560966984,0.914855231051352,1.00001234972447),
(1.00001522637195,0.91694597420133,1.00001204647505),(1.00001428784852,
0.922065259968872,1.00001130395417),(1.00001395123475,0.923901359098063,
1.00001103763929),(1.00001396081471,0.923849104111325,1.00001104521856),
(1.00001404571456,0.923386007914212,1.00001111238781),(1.00001437612857,
0.921583726099687,1.00001137379769),(1.00001462510049,0.92022567962924,
1.00001157077397),(1.00001558266985,0.915002505661038,1.00001232836319),
(1.000016489883,0.910054005470647,1.00001304611267),(1.0000187058405,0.897966806240904,
1.0000147992865),(1.000020028908,0.890749979859459,1.00001584604273),(1.00002292411146,
0.874957754155313,1.00001813660783),(1.00002451487478,0.866280749618104,
1.00001939515391),(1.00002619181141,0.857133702740162,1.00002072187673)))
REPRESENTATION_ITEM('')
SURFACE()
);
#469=(
BOUNDED_SURFACE()
B_SPLINE_SURFACE(3,2,((#31053,#31054,#31055),(#31056,#31057,#31058),(#31059,
#31060,#31061),(#31062,#31063,#31064),(#31065,#31066,#31067),(#31068,#31069,
#31070),(#31071,#31072,#31073),(#31074,#31075,#31076),(#31077,#31078,#31079),
(#31080,#31081,#31082),(#31083,#31084,#31085),(#31086,#31087,#31088),(#31089,
#31090,#31091),(#31092,#31093,#31094),(#31095,#31096,#31097),(#31098,#31099,
#31100),(#31101,#31102,#31103),(#31104,#31105,#31106)),.UNSPECIFIED.,.F.,
 .F.,.F.)
B_SPLINE_SURFACE_WITH_KNOTS((4,2,2,2,2,2,2,2,4),(3,3),(0.00330583080240977,
0.00509876127290382,0.00599522650815085,0.00689169174339787,0.00733992436102138,
0.0077881569786449,0.00868462221389192,0.00958108744913895,0.010477552684386),
(0.,1.),.UNSPECIFIED.)
GEOMETRIC_REPRESENTATION_ITEM()
RATIONAL_B_SPLINE_SURFACE(((1.,0.858051573205352,1.),(1.,0.875590740245157,
1.),(1.,0.891984535277027,1.),(1.,0.91012353548971,1.),(1.,0.915171726878721,
1.),(1.,0.922080092984699,1.),(1.,0.923887406775799,1.),(1.,0.923875556180464,
1.),(1.,0.923415662237299,1.),(1.,0.92160990901839,1.),(1.,0.920278779497093,
1.),(1.,0.915132747989307,1.),(1.,0.910082531829311,1.),(1.,0.897961000925736,
1.),(1.,0.890907866965291,1.),(1.,0.875336477322621,1.),(1.,0.866807510696485,
1.),(1.,0.858055143785041,1.)))
REPRESENTATION_ITEM('')
SURFACE()
);
#470=(
BOUNDED_SURFACE()
B_SPLINE_SURFACE(3,2,((#31335,#31336,#31337,#31338,#31339,#31340,#31341,
#31342,#31343,#31344,#31345,#31346,#31347,#31348,#31349,#31350,#31351,#31352,
#31353,#31354,#31355,#31356,#31357,#31358,#31359,#31360,#31361,#31362,#31363,
#31364,#31365,#31366,#31367,#31368,#31369,#31370,#31371,#31372,#31373,#31374,
#31375,#31376,#31377,#31378,#31379,#31380,#31381,#31382,#31383,#31384,#31385,
#31386,#31387,#31388,#31389,#31390,#31391,#31392,#31393,#31394,#31395,#31396,
#31397,#31398,#31399),(#31400,#31401,#31402,#31403,#31404,#31405,#31406,
#31407,#31408,#31409,#31410,#31411,#31412,#31413,#31414,#31415,#31416,#31417,
#31418,#31419,#31420,#31421,#31422,#31423,#31424,#31425,#31426,#31427,#31428,
#31429,#31430,#31431,#31432,#31433,#31434,#31435,#31436,#31437,#31438,#31439,
#31440,#31441,#31442,#31443,#31444,#31445,#31446,#31447,#31448,#31449,#31450,
#31451,#31452,#31453,#31454,#31455,#31456,#31457,#31458,#31459,#31460,#31461,
#31462,#31463,#31464),(#31465,#31466,#31467,#31468,#31469,#31470,#31471,
#31472,#31473,#31474,#31475,#31476,#31477,#31478,#31479,#31480,#31481,#31482,
#31483,#31484,#31485,#31486,#31487,#31488,#31489,#31490,#31491,#31492,#31493,
#31494,#31495,#31496,#31497,#31498,#31499,#31500,#31501,#31502,#31503,#31504,
#31505,#31506,#31507,#31508,#31509,#31510,#31511,#31512,#31513,#31514,#31515,
#31516,#31517,#31518,#31519,#31520,#31521,#31522,#31523,#31524,#31525,#31526,
#31527,#31528,#31529),(#31530,#31531,#31532,#31533,#31534,#31535,#31536,
#31537,#31538,#31539,#31540,#31541,#31542,#31543,#31544,#31545,#31546,#31547,
#31548,#31549,#31550,#31551,#31552,#31553,#31554,#31555,#31556,#31557,#31558,
#31559,#31560,#31561,#31562,#31563,#31564,#31565,#31566,#31567,#31568,#31569,
#31570,#31571,#31572,#31573,#31574,#31575,#31576,#31577,#31578,#31579,#31580,
#31581,#31582,#31583,#31584,#31585,#31586,#31587,#31588,#31589,#31590,#31591,
#31592,#31593,#31594)),.UNSPECIFIED.,.F.,.F.,.F.)
B_SPLINE_SURFACE_WITH_KNOTS((4,4),(3,2,2,2,2,2,2,2,2,2,2,2,2,2,2,2,2,2,
2,2,2,2,2,2,2,2,2,2,2,2,2,2,3),(0.,1.),(0.,0.03125,0.0625,0.09375,0.125,
0.15625,0.1875,0.21875,0.25,0.28125,0.3125,0.34375,0.375,0.40625,0.4375,
0.46875,0.5,0.53125,0.5625,0.59375,0.625,0.65625,0.6875,0.71875,0.75,0.78125,
0.8125,0.84375,0.875,0.90625,0.9375,0.96875,1.),.UNSPECIFIED.)
GEOMETRIC_REPRESENTATION_ITEM()
RATIONAL_B_SPLINE_SURFACE(((1.,0.923879532511287,1.,0.923879532511287,1.,
0.923879532511287,1.,0.923879532511287,1.,0.923879532511287,1.,0.923879532511287,
1.,0.923879532511287,1.,0.923879532511287,1.,0.923879532511287,1.,0.923879532511287,
1.,0.923879532511287,1.,0.923879532511287,1.,0.923879532511287,1.,0.923879532511287,
1.,0.923879532511287,1.,0.923879532511287,1.,0.923879532511287,1.,0.923879532511287,
1.,0.923879532511287,1.,0.923879532511287,1.,0.923879532511287,1.,0.923879532511287,
1.,0.923879532511287,1.,0.923879532511287,1.,0.923879532511287,1.,0.923879532511287,
1.,0.923879532511287,1.,0.923879532511287,1.,0.923879532511287,1.,0.923879532511287,
1.,0.923879532511287,1.,0.923879532511287,1.),(0.804737854124365,0.743480832462554,
0.804737854124365,0.743480832462554,0.804737854124365,0.743480832462554,
0.804737854124365,0.743480832462554,0.804737854124365,0.743480832462554,
0.804737854124365,0.743480832462554,0.804737854124365,0.743480832462554,
0.804737854124365,0.743480832462554,0.804737854124365,0.743480832462554,
0.804737854124365,0.743480832462554,0.804737854124365,0.743480832462554,
0.804737854124365,0.743480832462554,0.804737854124365,0.743480832462554,
0.804737854124365,0.743480832462554,0.804737854124365,0.743480832462554,
0.804737854124365,0.743480832462554,0.804737854124365,0.743480832462554,
0.804737854124365,0.743480832462554,0.804737854124365,0.743480832462554,
0.804737854124365,0.743480832462554,0.804737854124365,0.743480832462554,
0.804737854124365,0.743480832462554,0.804737854124365,0.743480832462554,
0.804737854124365,0.743480832462554,0.804737854124365,0.743480832462554,
0.804737854124365,0.743480832462554,0.804737854124365,0.743480832462554,
0.804737854124365,0.743480832462554,0.804737854124365,0.743480832462554,
0.804737854124365,0.743480832462554,0.804737854124365,0.743480832462554,
0.804737854124365,0.743480832462554,0.804737854124365),(0.804737854124365,
0.743480832462554,0.804737854124365,0.743480832462554,0.804737854124365,
0.743480832462554,0.804737854124365,0.743480832462554,0.804737854124365,
0.743480832462554,0.804737854124365,0.743480832462554,0.804737854124365,
0.743480832462554,0.804737854124365,0.743480832462554,0.804737854124365,
0.743480832462554,0.804737854124365,0.743480832462554,0.804737854124365,
0.743480832462554,0.804737854124365,0.743480832462554,0.804737854124365,
0.743480832462554,0.804737854124365,0.743480832462554,0.804737854124365,
0.743480832462554,0.804737854124365,0.743480832462554,0.804737854124365,
0.743480832462554,0.804737854124365,0.743480832462554,0.804737854124365,
0.743480832462554,0.804737854124365,0.743480832462554,0.804737854124365,
0.743480832462554,0.804737854124365,0.743480832462554,0.804737854124365,
0.743480832462554,0.804737854124365,0.743480832462554,0.804737854124365,
0.743480832462554,0.804737854124365,0.743480832462554,0.804737854124365,
0.743480832462554,0.804737854124365,0.743480832462554,0.804737854124365,
0.743480832462554,0.804737854124365,0.743480832462554,0.804737854124365,
0.743480832462554,0.804737854124365,0.743480832462554,0.804737854124365),
(1.,0.923879532511287,1.,0.923879532511287,1.,0.923879532511287,1.,0.923879532511287,
1.,0.923879532511287,1.,0.923879532511287,1.,0.923879532511287,1.,0.923879532511287,
1.,0.923879532511287,1.,0.923879532511287,1.,0.923879532511287,1.,0.923879532511287,
1.,0.923879532511287,1.,0.923879532511287,1.,0.923879532511287,1.,0.923879532511287,
1.,0.923879532511287,1.,0.923879532511287,1.,0.923879532511287,1.,0.923879532511287,
1.,0.923879532511287,1.,0.923879532511287,1.,0.923879532511287,1.,0.923879532511287,
1.,0.923879532511287,1.,0.923879532511287,1.,0.923879532511287,1.,0.923879532511287,
1.,0.923879532511287,1.,0.923879532511287,1.,0.923879532511287,1.,0.923879532511287,
1.)))
REPRESENTATION_ITEM('')
SURFACE()
);
#471=(
BOUNDED_SURFACE()
B_SPLINE_SURFACE(3,2,((#31733,#31734,#31735,#31736,#31737,#31738,#31739,
#31740,#31741,#31742,#31743,#31744,#31745,#31746,#31747,#31748,#31749,#31750,
#31751,#31752,#31753,#31754,#31755,#31756,#31757,#31758,#31759,#31760,#31761,
#31762,#31763,#31764,#31765,#31766,#31767,#31768,#31769,#31770,#31771,#31772,
#31773,#31774,#31775,#31776,#31777,#31778,#31779,#31780,#31781,#31782,#31783,
#31784,#31785,#31786,#31787,#31788,#31789,#31790,#31791,#31792,#31793,#31794,
#31795,#31796,#31797),(#31798,#31799,#31800,#31801,#31802,#31803,#31804,
#31805,#31806,#31807,#31808,#31809,#31810,#31811,#31812,#31813,#31814,#31815,
#31816,#31817,#31818,#31819,#31820,#31821,#31822,#31823,#31824,#31825,#31826,
#31827,#31828,#31829,#31830,#31831,#31832,#31833,#31834,#31835,#31836,#31837,
#31838,#31839,#31840,#31841,#31842,#31843,#31844,#31845,#31846,#31847,#31848,
#31849,#31850,#31851,#31852,#31853,#31854,#31855,#31856,#31857,#31858,#31859,
#31860,#31861,#31862),(#31863,#31864,#31865,#31866,#31867,#31868,#31869,
#31870,#31871,#31872,#31873,#31874,#31875,#31876,#31877,#31878,#31879,#31880,
#31881,#31882,#31883,#31884,#31885,#31886,#31887,#31888,#31889,#31890,#31891,
#31892,#31893,#31894,#31895,#31896,#31897,#31898,#31899,#31900,#31901,#31902,
#31903,#31904,#31905,#31906,#31907,#31908,#31909,#31910,#31911,#31912,#31913,
#31914,#31915,#31916,#31917,#31918,#31919,#31920,#31921,#31922,#31923,#31924,
#31925,#31926,#31927),(#31928,#31929,#31930,#31931,#31932,#31933,#31934,
#31935,#31936,#31937,#31938,#31939,#31940,#31941,#31942,#31943,#31944,#31945,
#31946,#31947,#31948,#31949,#31950,#31951,#31952,#31953,#31954,#31955,#31956,
#31957,#31958,#31959,#31960,#31961,#31962,#31963,#31964,#31965,#31966,#31967,
#31968,#31969,#31970,#31971,#31972,#31973,#31974,#31975,#31976,#31977,#31978,
#31979,#31980,#31981,#31982,#31983,#31984,#31985,#31986,#31987,#31988,#31989,
#31990,#31991,#31992)),.UNSPECIFIED.,.F.,.F.,.F.)
B_SPLINE_SURFACE_WITH_KNOTS((4,4),(3,2,2,2,2,2,2,2,2,2,2,2,2,2,2,2,2,2,
2,2,2,2,2,2,2,2,2,2,2,2,2,2,3),(0.,1.),(0.,0.03125,0.0625,0.09375,0.125,
0.15625,0.1875,0.21875,0.25,0.28125,0.3125,0.34375,0.375,0.40625,0.4375,
0.46875,0.5,0.53125,0.5625,0.59375,0.625,0.65625,0.6875,0.71875,0.75,0.78125,
0.8125,0.84375,0.875,0.90625,0.9375,0.96875,1.),.UNSPECIFIED.)
GEOMETRIC_REPRESENTATION_ITEM()
RATIONAL_B_SPLINE_SURFACE(((1.,0.923879532511287,1.,0.923879532511287,1.,
0.923879532511287,1.,0.923879532511287,1.,0.923879532511287,1.,0.923879532511287,
1.,0.923879532511287,1.,0.923879532511287,1.,0.923879532511287,1.,0.923879532511287,
1.,0.923879532511287,1.,0.923879532511287,1.,0.923879532511287,1.,0.923879532511287,
1.,0.923879532511287,1.,0.923879532511287,1.,0.923879532511287,1.,0.923879532511287,
1.,0.923879532511287,1.,0.923879532511287,1.,0.923879532511287,1.,0.923879532511287,
1.,0.923879532511287,1.,0.923879532511287,1.,0.923879532511287,1.,0.923879532511287,
1.,0.923879532511287,1.,0.923879532511287,1.,0.923879532511287,1.,0.923879532511287,
1.,0.923879532511287,1.,0.923879532511287,1.),(0.804737854124365,0.743480832462554,
0.804737854124365,0.743480832462554,0.804737854124365,0.743480832462554,
0.804737854124365,0.743480832462554,0.804737854124365,0.743480832462554,
0.804737854124365,0.743480832462554,0.804737854124365,0.743480832462554,
0.804737854124365,0.743480832462554,0.804737854124365,0.743480832462554,
0.804737854124365,0.743480832462554,0.804737854124365,0.743480832462554,
0.804737854124365,0.743480832462554,0.804737854124365,0.743480832462554,
0.804737854124365,0.743480832462554,0.804737854124365,0.743480832462554,
0.804737854124365,0.743480832462554,0.804737854124365,0.743480832462554,
0.804737854124365,0.743480832462554,0.804737854124365,0.743480832462554,
0.804737854124365,0.743480832462554,0.804737854124365,0.743480832462554,
0.804737854124365,0.743480832462554,0.804737854124365,0.743480832462554,
0.804737854124365,0.743480832462554,0.804737854124365,0.743480832462554,
0.804737854124365,0.743480832462554,0.804737854124365,0.743480832462554,
0.804737854124365,0.743480832462554,0.804737854124365,0.743480832462554,
0.804737854124365,0.743480832462554,0.804737854124365,0.743480832462554,
0.804737854124365,0.743480832462554,0.804737854124365),(0.804737854124365,
0.743480832462554,0.804737854124365,0.743480832462554,0.804737854124365,
0.743480832462554,0.804737854124365,0.743480832462554,0.804737854124365,
0.743480832462554,0.804737854124365,0.743480832462554,0.804737854124365,
0.743480832462554,0.804737854124365,0.743480832462554,0.804737854124365,
0.743480832462554,0.804737854124365,0.743480832462554,0.804737854124365,
0.743480832462554,0.804737854124365,0.743480832462554,0.804737854124365,
0.743480832462554,0.804737854124365,0.743480832462554,0.804737854124365,
0.743480832462554,0.804737854124365,0.743480832462554,0.804737854124365,
0.743480832462554,0.804737854124365,0.743480832462554,0.804737854124365,
0.743480832462554,0.804737854124365,0.743480832462554,0.804737854124365,
0.743480832462554,0.804737854124365,0.743480832462554,0.804737854124365,
0.743480832462554,0.804737854124365,0.743480832462554,0.804737854124365,
0.743480832462554,0.804737854124365,0.743480832462554,0.804737854124365,
0.743480832462554,0.804737854124365,0.743480832462554,0.804737854124365,
0.743480832462554,0.804737854124365,0.743480832462554,0.804737854124365,
0.743480832462554,0.804737854124365,0.743480832462554,0.804737854124365),
(1.,0.923879532511287,1.,0.923879532511287,1.,0.923879532511287,1.,0.923879532511287,
1.,0.923879532511287,1.,0.923879532511287,1.,0.923879532511287,1.,0.923879532511287,
1.,0.923879532511287,1.,0.923879532511287,1.,0.923879532511287,1.,0.923879532511287,
1.,0.923879532511287,1.,0.923879532511287,1.,0.923879532511287,1.,0.923879532511287,
1.,0.923879532511287,1.,0.923879532511287,1.,0.923879532511287,1.,0.923879532511287,
1.,0.923879532511287,1.,0.923879532511287,1.,0.923879532511287,1.,0.923879532511287,
1.,0.923879532511287,1.,0.923879532511287,1.,0.923879532511287,1.,0.923879532511287,
1.,0.923879532511287,1.,0.923879532511287,1.,0.923879532511287,1.,0.923879532511287,
1.)))
REPRESENTATION_ITEM('')
SURFACE()
);
#472=(
BOUNDED_SURFACE()
B_SPLINE_SURFACE(3,2,((#32062,#32063,#32064,#32065,#32066,#32067,#32068,
#32069,#32070,#32071,#32072,#32073,#32074,#32075,#32076,#32077,#32078,#32079,
#32080,#32081,#32082,#32083,#32084,#32085,#32086,#32087,#32088,#32089,#32090,
#32091,#32092,#32093,#32094,#32095,#32096,#32097,#32098,#32099,#32100,#32101,
#32102,#32103,#32104,#32105,#32106,#32107,#32108,#32109,#32110,#32111,#32112,
#32113,#32114,#32115,#32116,#32117,#32118,#32119,#32120,#32121,#32122,#32123,
#32124,#32125,#32126),(#32127,#32128,#32129,#32130,#32131,#32132,#32133,
#32134,#32135,#32136,#32137,#32138,#32139,#32140,#32141,#32142,#32143,#32144,
#32145,#32146,#32147,#32148,#32149,#32150,#32151,#32152,#32153,#32154,#32155,
#32156,#32157,#32158,#32159,#32160,#32161,#32162,#32163,#32164,#32165,#32166,
#32167,#32168,#32169,#32170,#32171,#32172,#32173,#32174,#32175,#32176,#32177,
#32178,#32179,#32180,#32181,#32182,#32183,#32184,#32185,#32186,#32187,#32188,
#32189,#32190,#32191),(#32192,#32193,#32194,#32195,#32196,#32197,#32198,
#32199,#32200,#32201,#32202,#32203,#32204,#32205,#32206,#32207,#32208,#32209,
#32210,#32211,#32212,#32213,#32214,#32215,#32216,#32217,#32218,#32219,#32220,
#32221,#32222,#32223,#32224,#32225,#32226,#32227,#32228,#32229,#32230,#32231,
#32232,#32233,#32234,#32235,#32236,#32237,#32238,#32239,#32240,#32241,#32242,
#32243,#32244,#32245,#32246,#32247,#32248,#32249,#32250,#32251,#32252,#32253,
#32254,#32255,#32256),(#32257,#32258,#32259,#32260,#32261,#32262,#32263,
#32264,#32265,#32266,#32267,#32268,#32269,#32270,#32271,#32272,#32273,#32274,
#32275,#32276,#32277,#32278,#32279,#32280,#32281,#32282,#32283,#32284,#32285,
#32286,#32287,#32288,#32289,#32290,#32291,#32292,#32293,#32294,#32295,#32296,
#32297,#32298,#32299,#32300,#32301,#32302,#32303,#32304,#32305,#32306,#32307,
#32308,#32309,#32310,#32311,#32312,#32313,#32314,#32315,#32316,#32317,#32318,
#32319,#32320,#32321)),.UNSPECIFIED.,.F.,.F.,.F.)
B_SPLINE_SURFACE_WITH_KNOTS((4,4),(3,2,2,2,2,2,2,2,2,2,2,2,2,2,2,2,2,2,
2,2,2,2,2,2,2,2,2,2,2,2,2,2,3),(0.,1.),(0.,0.03125,0.0625,0.09375,0.125,
0.15625,0.1875,0.21875,0.25,0.28125,0.3125,0.34375,0.375,0.40625,0.4375,
0.46875,0.5,0.53125,0.5625,0.59375,0.625,0.65625,0.6875,0.71875,0.75,0.78125,
0.8125,0.84375,0.875,0.90625,0.9375,0.96875,1.),.UNSPECIFIED.)
GEOMETRIC_REPRESENTATION_ITEM()
RATIONAL_B_SPLINE_SURFACE(((1.,0.923879532511287,1.,0.923879532511287,1.,
0.923879532511287,1.,0.923879532511287,1.,0.923879532511287,1.,0.923879532511287,
1.,0.923879532511287,1.,0.923879532511287,1.,0.923879532511287,1.,0.923879532511287,
1.,0.923879532511287,1.,0.923879532511287,1.,0.923879532511287,1.,0.923879532511287,
1.,0.923879532511287,1.,0.923879532511287,1.,0.923879532511287,1.,0.923879532511287,
1.,0.923879532511287,1.,0.923879532511287,1.,0.923879532511287,1.,0.923879532511287,
1.,0.923879532511287,1.,0.923879532511287,1.,0.923879532511287,1.,0.923879532511287,
1.,0.923879532511287,1.,0.923879532511287,1.,0.923879532511287,1.,0.923879532511287,
1.,0.923879532511287,1.,0.923879532511287,1.),(0.804737854124365,0.743480832462554,
0.804737854124365,0.743480832462554,0.804737854124365,0.743480832462554,
0.804737854124365,0.743480832462554,0.804737854124365,0.743480832462554,
0.804737854124365,0.743480832462554,0.804737854124365,0.743480832462554,
0.804737854124365,0.743480832462554,0.804737854124365,0.743480832462554,
0.804737854124365,0.743480832462554,0.804737854124365,0.743480832462554,
0.804737854124365,0.743480832462554,0.804737854124365,0.743480832462554,
0.804737854124365,0.743480832462554,0.804737854124365,0.743480832462554,
0.804737854124365,0.743480832462554,0.804737854124365,0.743480832462554,
0.804737854124365,0.743480832462554,0.804737854124365,0.743480832462554,
0.804737854124365,0.743480832462554,0.804737854124365,0.743480832462554,
0.804737854124365,0.743480832462554,0.804737854124365,0.743480832462554,
0.804737854124365,0.743480832462554,0.804737854124365,0.743480832462554,
0.804737854124365,0.743480832462554,0.804737854124365,0.743480832462554,
0.804737854124365,0.743480832462554,0.804737854124365,0.743480832462554,
0.804737854124365,0.743480832462554,0.804737854124365,0.743480832462554,
0.804737854124365,0.743480832462554,0.804737854124365),(0.804737854124365,
0.743480832462554,0.804737854124365,0.743480832462554,0.804737854124365,
0.743480832462554,0.804737854124365,0.743480832462554,0.804737854124365,
0.743480832462554,0.804737854124365,0.743480832462554,0.804737854124365,
0.743480832462554,0.804737854124365,0.743480832462554,0.804737854124365,
0.743480832462554,0.804737854124365,0.743480832462554,0.804737854124365,
0.743480832462554,0.804737854124365,0.743480832462554,0.804737854124365,
0.743480832462554,0.804737854124365,0.743480832462554,0.804737854124365,
0.743480832462554,0.804737854124365,0.743480832462554,0.804737854124365,
0.743480832462554,0.804737854124365,0.743480832462554,0.804737854124365,
0.743480832462554,0.804737854124365,0.743480832462554,0.804737854124365,
0.743480832462554,0.804737854124365,0.743480832462554,0.804737854124365,
0.743480832462554,0.804737854124365,0.743480832462554,0.804737854124365,
0.743480832462554,0.804737854124365,0.743480832462554,0.804737854124365,
0.743480832462554,0.804737854124365,0.743480832462554,0.804737854124365,
0.743480832462554,0.804737854124365,0.743480832462554,0.804737854124365,
0.743480832462554,0.804737854124365,0.743480832462554,0.804737854124365),
(1.,0.923879532511287,1.,0.923879532511287,1.,0.923879532511287,1.,0.923879532511287,
1.,0.923879532511287,1.,0.923879532511287,1.,0.923879532511287,1.,0.923879532511287,
1.,0.923879532511287,1.,0.923879532511287,1.,0.923879532511287,1.,0.923879532511287,
1.,0.923879532511287,1.,0.923879532511287,1.,0.923879532511287,1.,0.923879532511287,
1.,0.923879532511287,1.,0.923879532511287,1.,0.923879532511287,1.,0.923879532511287,
1.,0.923879532511287,1.,0.923879532511287,1.,0.923879532511287,1.,0.923879532511287,
1.,0.923879532511287,1.,0.923879532511287,1.,0.923879532511287,1.,0.923879532511287,
1.,0.923879532511287,1.,0.923879532511287,1.,0.923879532511287,1.,0.923879532511287,
1.)))
REPRESENTATION_ITEM('')
SURFACE()
);
#473=(
BOUNDED_SURFACE()
B_SPLINE_SURFACE(3,2,((#32391,#32392,#32393,#32394,#32395,#32396,#32397,
#32398,#32399,#32400,#32401,#32402,#32403,#32404,#32405,#32406,#32407,#32408,
#32409,#32410,#32411,#32412,#32413,#32414,#32415,#32416,#32417,#32418,#32419,
#32420,#32421,#32422,#32423,#32424,#32425,#32426,#32427,#32428,#32429,#32430,
#32431,#32432,#32433,#32434,#32435,#32436,#32437,#32438,#32439,#32440,#32441,
#32442,#32443,#32444,#32445,#32446,#32447,#32448,#32449,#32450,#32451,#32452,
#32453,#32454,#32455),(#32456,#32457,#32458,#32459,#32460,#32461,#32462,
#32463,#32464,#32465,#32466,#32467,#32468,#32469,#32470,#32471,#32472,#32473,
#32474,#32475,#32476,#32477,#32478,#32479,#32480,#32481,#32482,#32483,#32484,
#32485,#32486,#32487,#32488,#32489,#32490,#32491,#32492,#32493,#32494,#32495,
#32496,#32497,#32498,#32499,#32500,#32501,#32502,#32503,#32504,#32505,#32506,
#32507,#32508,#32509,#32510,#32511,#32512,#32513,#32514,#32515,#32516,#32517,
#32518,#32519,#32520),(#32521,#32522,#32523,#32524,#32525,#32526,#32527,
#32528,#32529,#32530,#32531,#32532,#32533,#32534,#32535,#32536,#32537,#32538,
#32539,#32540,#32541,#32542,#32543,#32544,#32545,#32546,#32547,#32548,#32549,
#32550,#32551,#32552,#32553,#32554,#32555,#32556,#32557,#32558,#32559,#32560,
#32561,#32562,#32563,#32564,#32565,#32566,#32567,#32568,#32569,#32570,#32571,
#32572,#32573,#32574,#32575,#32576,#32577,#32578,#32579,#32580,#32581,#32582,
#32583,#32584,#32585),(#32586,#32587,#32588,#32589,#32590,#32591,#32592,
#32593,#32594,#32595,#32596,#32597,#32598,#32599,#32600,#32601,#32602,#32603,
#32604,#32605,#32606,#32607,#32608,#32609,#32610,#32611,#32612,#32613,#32614,
#32615,#32616,#32617,#32618,#32619,#32620,#32621,#32622,#32623,#32624,#32625,
#32626,#32627,#32628,#32629,#32630,#32631,#32632,#32633,#32634,#32635,#32636,
#32637,#32638,#32639,#32640,#32641,#32642,#32643,#32644,#32645,#32646,#32647,
#32648,#32649,#32650)),.UNSPECIFIED.,.F.,.F.,.F.)
B_SPLINE_SURFACE_WITH_KNOTS((4,4),(3,2,2,2,2,2,2,2,2,2,2,2,2,2,2,2,2,2,
2,2,2,2,2,2,2,2,2,2,2,2,2,2,3),(0.,1.),(0.,0.03125,0.0625,0.09375,0.125,
0.15625,0.1875,0.21875,0.25,0.28125,0.3125,0.34375,0.375,0.40625,0.4375,
0.46875,0.5,0.53125,0.5625,0.59375,0.625,0.65625,0.6875,0.71875,0.75,0.78125,
0.8125,0.84375,0.875,0.90625,0.9375,0.96875,1.),.UNSPECIFIED.)
GEOMETRIC_REPRESENTATION_ITEM()
RATIONAL_B_SPLINE_SURFACE(((1.,0.923879532511287,1.,0.923879532511287,1.,
0.923879532511287,1.,0.923879532511287,1.,0.923879532511287,1.,0.923879532511287,
1.,0.923879532511287,1.,0.923879532511287,1.,0.923879532511287,1.,0.923879532511287,
1.,0.923879532511287,1.,0.923879532511287,1.,0.923879532511287,1.,0.923879532511287,
1.,0.923879532511287,1.,0.923879532511287,1.,0.923879532511287,1.,0.923879532511287,
1.,0.923879532511287,1.,0.923879532511287,1.,0.923879532511287,1.,0.923879532511287,
1.,0.923879532511287,1.,0.923879532511287,1.,0.923879532511287,1.,0.923879532511287,
1.,0.923879532511287,1.,0.923879532511287,1.,0.923879532511287,1.,0.923879532511287,
1.,0.923879532511287,1.,0.923879532511287,1.),(0.804737854124365,0.743480832462554,
0.804737854124365,0.743480832462554,0.804737854124365,0.743480832462554,
0.804737854124365,0.743480832462554,0.804737854124365,0.743480832462554,
0.804737854124365,0.743480832462554,0.804737854124365,0.743480832462554,
0.804737854124365,0.743480832462554,0.804737854124365,0.743480832462554,
0.804737854124365,0.743480832462554,0.804737854124365,0.743480832462554,
0.804737854124365,0.743480832462554,0.804737854124365,0.743480832462554,
0.804737854124365,0.743480832462554,0.804737854124365,0.743480832462554,
0.804737854124365,0.743480832462554,0.804737854124365,0.743480832462554,
0.804737854124365,0.743480832462554,0.804737854124365,0.743480832462554,
0.804737854124365,0.743480832462554,0.804737854124365,0.743480832462554,
0.804737854124365,0.743480832462554,0.804737854124365,0.743480832462554,
0.804737854124365,0.743480832462554,0.804737854124365,0.743480832462554,
0.804737854124365,0.743480832462554,0.804737854124365,0.743480832462554,
0.804737854124365,0.743480832462554,0.804737854124365,0.743480832462554,
0.804737854124365,0.743480832462554,0.804737854124365,0.743480832462554,
0.804737854124365,0.743480832462554,0.804737854124365),(0.804737854124365,
0.743480832462554,0.804737854124365,0.743480832462554,0.804737854124365,
0.743480832462554,0.804737854124365,0.743480832462554,0.804737854124365,
0.743480832462554,0.804737854124365,0.743480832462554,0.804737854124365,
0.743480832462554,0.804737854124365,0.743480832462554,0.804737854124365,
0.743480832462554,0.804737854124365,0.743480832462554,0.804737854124365,
0.743480832462554,0.804737854124365,0.743480832462554,0.804737854124365,
0.743480832462554,0.804737854124365,0.743480832462554,0.804737854124365,
0.743480832462554,0.804737854124365,0.743480832462554,0.804737854124365,
0.743480832462554,0.804737854124365,0.743480832462554,0.804737854124365,
0.743480832462554,0.804737854124365,0.743480832462554,0.804737854124365,
0.743480832462554,0.804737854124365,0.743480832462554,0.804737854124365,
0.743480832462554,0.804737854124365,0.743480832462554,0.804737854124365,
0.743480832462554,0.804737854124365,0.743480832462554,0.804737854124365,
0.743480832462554,0.804737854124365,0.743480832462554,0.804737854124365,
0.743480832462554,0.804737854124365,0.743480832462554,0.804737854124365,
0.743480832462554,0.804737854124365,0.743480832462554,0.804737854124365),
(1.,0.923879532511287,1.,0.923879532511287,1.,0.923879532511287,1.,0.923879532511287,
1.,0.923879532511287,1.,0.923879532511287,1.,0.923879532511287,1.,0.923879532511287,
1.,0.923879532511287,1.,0.923879532511287,1.,0.923879532511287,1.,0.923879532511287,
1.,0.923879532511287,1.,0.923879532511287,1.,0.923879532511287,1.,0.923879532511287,
1.,0.923879532511287,1.,0.923879532511287,1.,0.923879532511287,1.,0.923879532511287,
1.,0.923879532511287,1.,0.923879532511287,1.,0.923879532511287,1.,0.923879532511287,
1.,0.923879532511287,1.,0.923879532511287,1.,0.923879532511287,1.,0.923879532511287,
1.,0.923879532511287,1.,0.923879532511287,1.,0.923879532511287,1.,0.923879532511287,
1.)))
REPRESENTATION_ITEM('')
SURFACE()
);
#474=FACE_BOUND('',#1698,.T.);
#475=FACE_BOUND('',#1700,.T.);
#476=FACE_BOUND('',#1710,.T.);
#477=FACE_BOUND('',#1722,.T.);
#478=FACE_BOUND('',#1725,.T.);
#479=FACE_BOUND('',#1726,.T.);
#480=FACE_BOUND('',#1731,.T.);
#481=FACE_BOUND('',#1744,.T.);
#482=FACE_BOUND('',#1748,.T.);
#483=FACE_BOUND('',#1751,.T.);
#484=FACE_BOUND('',#1754,.T.);
#485=FACE_BOUND('',#1755,.T.);
#486=FACE_BOUND('',#1757,.T.);
#487=FACE_BOUND('',#1760,.T.);
#488=FACE_BOUND('',#1762,.T.);
#489=FACE_BOUND('',#1768,.T.);
#490=FACE_BOUND('',#1772,.T.);
#491=FACE_BOUND('',#1786,.T.);
#492=FACE_BOUND('',#1788,.T.);
#493=FACE_BOUND('',#1815,.T.);
#494=FACE_BOUND('',#1817,.T.);
#495=FACE_BOUND('',#1820,.T.);
#496=FACE_BOUND('',#1849,.T.);
#497=FACE_BOUND('',#1850,.T.);
#498=FACE_BOUND('',#1851,.T.);
#499=FACE_BOUND('',#1852,.T.);
#500=FACE_BOUND('',#1853,.T.);
#501=FACE_BOUND('',#1854,.T.);
#502=FACE_BOUND('',#1855,.T.);
#503=FACE_BOUND('',#1856,.T.);
#504=FACE_BOUND('',#1857,.T.);
#505=FACE_BOUND('',#1859,.T.);
#506=FACE_BOUND('',#1861,.T.);
#507=FACE_BOUND('',#1863,.T.);
#508=FACE_BOUND('',#1865,.T.);
#509=FACE_BOUND('',#1867,.T.);
#510=FACE_BOUND('',#1868,.T.);
#511=FACE_BOUND('',#1912,.T.);
#512=FACE_BOUND('',#1914,.T.);
#513=FACE_BOUND('',#1916,.T.);
#514=FACE_BOUND('',#1923,.T.);
#515=FACE_BOUND('',#1926,.T.);
#516=FACE_BOUND('',#1939,.T.);
#517=FACE_BOUND('',#1947,.T.);
#518=FACE_BOUND('',#1949,.T.);
#519=FACE_BOUND('',#1952,.T.);
#520=FACE_BOUND('',#1961,.T.);
#521=FACE_BOUND('',#1967,.T.);
#522=FACE_BOUND('',#2001,.T.);
#523=FACE_BOUND('',#2003,.T.);
#524=FACE_BOUND('',#2008,.T.);
#525=FACE_BOUND('',#2012,.T.);
#526=FACE_BOUND('',#2015,.T.);
#527=FACE_BOUND('',#2028,.T.);
#528=FACE_BOUND('',#2033,.T.);
#529=FACE_BOUND('',#2036,.T.);
#530=FACE_BOUND('',#2037,.T.);
#531=FACE_BOUND('',#2038,.T.);
#532=FACE_BOUND('',#2039,.T.);
#533=FACE_BOUND('',#2040,.T.);
#534=FACE_BOUND('',#2042,.T.);
#535=FACE_BOUND('',#2046,.T.);
#536=FACE_BOUND('',#2048,.T.);
#537=FACE_BOUND('',#2049,.T.);
#538=FACE_BOUND('',#2050,.T.);
#539=FACE_BOUND('',#2051,.T.);
#540=FACE_BOUND('',#2052,.T.);
#541=FACE_BOUND('',#2061,.T.);
#542=FACE_BOUND('',#2064,.T.);
#543=FACE_BOUND('',#2116,.T.);
#544=FACE_BOUND('',#2118,.T.);
#545=FACE_BOUND('',#2128,.T.);
#546=FACE_BOUND('',#2157,.T.);
#547=FACE_BOUND('',#2162,.T.);
#548=FACE_BOUND('',#2165,.T.);
#549=FACE_BOUND('',#2172,.T.);
#550=FACE_BOUND('',#2179,.T.);
#551=FACE_BOUND('',#2187,.T.);
#552=FACE_BOUND('',#2190,.T.);
#553=FACE_BOUND('',#2192,.T.);
#554=B_SPLINE_CURVE_WITH_KNOTS('',3,(#14640,#14641,#14642,#14643,#14644,
#14645,#14646,#14647,#14648,#14649,#14650,#14651,#14652,#14653,#14654,#14655,
#14656,#14657,#14658,#14659,#14660,#14661,#14662,#14663,#14664,#14665,#14666,
#14667,#14668,#14669,#14670,#14671,#14672,#14673),.UNSPECIFIED.,.F.,.F.,
(4,3,3,3,3,3,3,3,3,3,3,4),(0.0010057065754485,0.00361866511599219,0.00531965656119927,
0.00803958816950913,0.010759519777819,0.0107707078352687,0.011882063272691,
0.0121325673456277,0.01349922673087,0.0162115567860829,0.0188836740964046,
0.0205357090950889),.UNSPECIFIED.);
#555=B_SPLINE_CURVE_WITH_KNOTS('',3,(#14677,#14678,#14679,#14680,#14681,
#14682,#14683,#14684,#14685,#14686,#14687,#14688,#14689,#14690,#14691,#14692,
#14693,#14694,#14695,#14696,#14697,#14698,#14699,#14700,#14701,#14702,#14703,
#14704,#14705,#14706,#14707,#14708,#14709,#14710),.UNSPECIFIED.,.F.,.F.,
(4,3,3,3,3,3,3,3,3,3,3,4),(0.00100601928210048,0.00367908692095566,0.00533170946801007,
0.00804500415847367,0.00941214959364056,0.0105239002825655,0.0107744934468549,
0.0107856854833192,0.013506584430358,0.0162274833773967,0.0188413712147584,
0.0205429676116094),.UNSPECIFIED.);
#556=B_SPLINE_CURVE_WITH_KNOTS('',3,(#14715,#14716,#14717,#14718),
 .UNSPECIFIED.,.F.,.F.,(4,4),(0.,0.00310259288128586),.UNSPECIFIED.);
#557=B_SPLINE_CURVE_WITH_KNOTS('',3,(#14720,#14721,#14722,#14723,#14724,
#14725,#14726,#14727,#14728,#14729,#14730,#14731,#14732,#14733,#14734,#14735,
#14736,#14737,#14738,#14739,#14740,#14741,#14742,#14743,#14744,#14745,#14746,
#14747,#14748,#14749,#14750,#14751,#14752,#14753,#14754,#14755,#14756,#14757,
#14758,#14759,#14760,#14761,#14762,#14763,#14764,#14765,#14766,#14767,#14768,
#14769,#14770,#14771,#14772,#14773,#14774,#14775,#14776,#14777,#14778,#14779,
#14780,#14781,#14782,#14783,#14784,#14785,#14786,#14787,#14788,#14789,#14790,
#14791,#14792,#14793,#14794,#14795,#14796,#14797,#14798),.UNSPECIFIED.,
 .F.,.F.,(4,3,3,3,3,3,3,3,3,3,3,3,3,3,3,3,3,3,3,3,3,3,3,3,3,3,4),(0.,0.00029089201195018,
0.00058177691126932,0.00116064017748705,0.001163542589709,0.00232128035497411,
0.00232708521749185,0.00464256070994822,0.00465417035496075,0.00696384106492234,
0.00698125566896419,0.00813318854443032,0.00928512141989645,0.00930822641010844,
0.0103189114251322,0.0113354153193445,0.0116064017748706,0.0127670419523576,
0.0139276821298447,0.0139287558918501,0.0148713512522913,0.0158107627881495,
0.0162438817323399,0.0162489624848188,0.0180760281528238,0.0183987634801277,
0.0185702428397929),.UNSPECIFIED.);
#558=B_SPLINE_CURVE_WITH_KNOTS('',3,(#14800,#14801,#14802,#14803,#14804,
#14805,#14806,#14807,#14808,#14809,#14810,#14811,#14812,#14813,#14814,#14815,
#14816,#14817,#14818,#14819,#14820,#14821,#14822,#14823,#14824,#14825,#14826,
#14827,#14828,#14829,#14830,#14831,#14832,#14833,#14834,#14835,#14836,#14837,
#14838,#14839,#14840,#14841,#14842,#14843,#14844,#14845,#14846,#14847,#14848,
#14849,#14850,#14851,#14852,#14853,#14854,#14855,#14856,#14857,#14858,#14859,
#14860,#14861,#14862,#14863),.UNSPECIFIED.,.F.,.F.,(4,3,3,3,3,3,3,3,3,3,
3,3,3,3,3,3,3,3,3,3,3,4),(-4.46439725195681E-5,0.00185117245303053,0.00227381448108523,
0.00415828625857787,0.00459227293469002,0.00459331693554309,0.00665251407402816,
0.00868942277861947,0.00922918984189961,0.00923169636203958,0.0115471745933297,
0.0115476482955044,0.0128084107178559,0.0138639458401943,0.0138661067491092,
0.016183484747819,0.016184565202714,0.0173432542021003,0.0173437944295164,
0.0179231270235531,0.0182130679058979,0.0185030236563188),.UNSPECIFIED.);
#559=B_SPLINE_CURVE_WITH_KNOTS('',3,(#14865,#14866,#14867,#14868),
 .UNSPECIFIED.,.F.,.F.,(4,4),(0.,0.00310259288126633),.UNSPECIFIED.);
#560=B_SPLINE_CURVE_WITH_KNOTS('',3,(#14875,#14876,#14877,#14878),
 .UNSPECIFIED.,.F.,.F.,(4,4),(0.,0.00310259288126371),.UNSPECIFIED.);
#561=B_SPLINE_CURVE_WITH_KNOTS('',3,(#14880,#14881,#14882,#14883,#14884,
#14885,#14886,#14887,#14888,#14889,#14890,#14891,#14892,#14893,#14894,#14895,
#14896,#14897,#14898,#14899,#14900,#14901,#14902,#14903,#14904,#14905,#14906,
#14907,#14908,#14909,#14910,#14911,#14912,#14913,#14914,#14915,#14916,#14917,
#14918,#14919,#14920,#14921,#14922,#14923,#14924,#14925,#14926,#14927,#14928,
#14929,#14930,#14931,#14932,#14933,#14934,#14935,#14936,#14937,#14938,#14939,
#14940,#14941,#14942,#14943,#14944,#14945,#14946,#14947,#14948,#14949,#14950,
#14951,#14952,#14953,#14954,#14955,#14956,#14957,#14958,#14959,#14960,#14961,
#14962,#14963,#14964,#14965,#14966,#14967),.UNSPECIFIED.,.F.,.F.,(4,3,3,
3,3,3,3,3,3,3,3,3,3,3,3,3,3,3,3,3,3,3,3,3,3,3,3,3,3,4),(0.,0.000288594368059549,
0.000577175639970858,0.00114871783547251,0.00115433020342524,0.00229743567094501,
0.00230866043814268,0.00359206730237028,0.00459487134189001,0.00461731070067686,
0.00543466283320275,0.00627129552525818,0.00689230701283501,0.00691299933338874,
0.00918974268378,0.00920315969262419,0.0101295449954259,0.01105604718127,
0.011487178354725,0.0114986296353845,0.01378461402567,0.0137972845775347,
0.0148523132937294,0.0158566070086,0.016082049696615,0.0172307675320875,
0.0176563774300653,0.0178051264498237,0.0180923059086919,0.01837948536756),
 .UNSPECIFIED.);
#562=B_SPLINE_CURVE_WITH_KNOTS('',3,(#14969,#14970,#14971,#14972,#14973,
#14974,#14975,#14976,#14977,#14978,#14979,#14980,#14981,#14982,#14983,#14984,
#14985,#14986,#14987,#14988,#14989,#14990,#14991,#14992,#14993,#14994,#14995,
#14996,#14997,#14998,#14999,#15000,#15001,#15002,#15003,#15004,#15005,#15006,
#15007,#15008,#15009,#15010,#15011,#15012,#15013,#15014,#15015,#15016,#15017,
#15018,#15019,#15020,#15021,#15022,#15023,#15024,#15025,#15026,#15027,#15028,
#15029,#15030,#15031,#15032),.UNSPECIFIED.,.F.,.F.,(4,3,3,3,3,3,3,3,3,3,
3,3,3,3,3,3,3,3,3,3,3,4),(-4.46439725204971E-5,0.00185117246158491,0.00227381448108429,
0.0041582862784131,0.00459227293468908,0.00459331693554219,0.00665251407724604,
0.00868942278715934,0.00922918984189866,0.00923169636203865,0.0115471745933288,
0.0115476482955035,0.0128084107214943,0.0138639458401934,0.0138661067491082,
0.016183484747818,0.016184565202713,0.0173432542020993,0.0173437944295154,
0.0179231270235523,0.0182130679058973,0.0185030236563178),.UNSPECIFIED.);
#563=B_SPLINE_CURVE_WITH_KNOTS('',3,(#15033,#15034,#15035,#15036),
 .UNSPECIFIED.,.F.,.F.,(4,4),(0.,0.00310259288126471),.UNSPECIFIED.);
#564=B_SPLINE_CURVE_WITH_KNOTS('',3,(#15045,#15046,#15047,#15048,#15049,
#15050,#15051,#15052,#15053,#15054,#15055,#15056,#15057,#15058,#15059,#15060,
#15061,#15062,#15063,#15064,#15065,#15066,#15067,#15068,#15069,#15070,#15071,
#15072,#15073,#15074,#15075,#15076,#15077,#15078,#15079,#15080,#15081,#15082,
#15083,#15084,#15085,#15086,#15087,#15088,#15089,#15090,#15091,#15092,#15093,
#15094,#15095,#15096),.UNSPECIFIED.,.F.,.F.,(4,3,3,3,3,3,3,3,3,3,3,3,3,
3,3,3,3,4),(0.00277080264391651,0.00293212141733799,0.00306062177311605,
0.0031161226260969,0.00324851187334901,0.00335821405905974,0.003462358473441,
0.00364274939856266,0.00382880230054904,0.00399591545353225,0.0041548301681292,
0.00436143559541393,0.00457232483906153,0.00478955939058047,0.0048473018628174,
0.00507782428691642,0.00531647499823543,0.0055397735575056),
 .UNSPECIFIED.);
#565=B_SPLINE_CURVE_WITH_KNOTS('',3,(#15097,#15098,#15099,#15100,#15101,
#15102,#15103,#15104,#15105,#15106,#15107,#15108,#15109,#15110,#15111,#15112,
#15113,#15114,#15115,#15116,#15117,#15118,#15119,#15120,#15121,#15122,#15123,
#15124,#15125,#15126,#15127,#15128,#15129,#15130,#15131,#15132,#15133,#15134,
#15135,#15136,#15137,#15138,#15139,#15140,#15141,#15142,#15143,#15144,#15145,
#15146,#15147,#15148,#15149,#15150,#15151,#15152,#15153,#15154,#15155,#15156,
#15157,#15158,#15159,#15160,#15161,#15162,#15163,#15164,#15165,#15166,#15167,
#15168,#15169,#15170,#15171,#15172,#15173,#15174,#15175,#15176,#15177,#15178,
#15179,#15180,#15181,#15182,#15183,#15184,#15185,#15186,#15187,#15188,#15189,
#15190,#15191,#15192,#15193,#15194,#15195,#15196,#15197,#15198,#15199,#15200,
#15201,#15202,#15203,#15204,#15205,#15206,#15207,#15208,#15209,#15210,#15211,
#15212,#15213,#15214,#15215,#15216,#15217,#15218,#15219,#15220,#15221,#15222,
#15223,#15224,#15225,#15226,#15227,#15228,#15229,#15230,#15231,#15232,#15233,
#15234,#15235,#15236,#15237,#15238,#15239,#15240,#15241,#15242,#15243,#15244,
#15245,#15246,#15247,#15248,#15249,#15250,#15251,#15252,#15253,#15254,#15255,
#15256,#15257,#15258,#15259,#15260,#15261,#15262,#15263,#15264,#15265,#15266,
#15267,#15268,#15269,#15270,#15271,#15272,#15273,#15274,#15275,#15276,#15277,
#15278,#15279,#15280,#15281,#15282,#15283,#15284,#15285,#15286,#15287,#15288,
#15289,#15290,#15291,#15292,#15293,#15294,#15295,#15296,#15297,#15298),
 .UNSPECIFIED.,.F.,.F.,(4,3,3,3,3,3,3,3,3,3,3,3,3,3,3,3,3,3,3,3,3,3,3,3,
3,3,3,3,3,3,3,3,3,3,3,3,3,3,3,3,3,3,3,3,3,3,3,3,3,3,3,3,3,3,3,3,3,3,3,3,
3,3,3,3,3,3,3,4),(0.,0.000340175691735185,0.000675474340953183,0.00101808855394696,
0.00136070276694074,0.00167669716890443,0.00171086518500347,0.00196577589295814,
0.00226595430547292,0.00252797514521974,0.00256629777750519,0.00286050548522501,
0.00299401407375605,0.0031748036777214,0.00335423798418269,0.00342173037000691,
0.00408388793721925,0.00427716296250863,0.00444284813951019,0.00452758478188326,
0.00469321101548466,0.00470487925875949,0.00501526856889436,0.00513259555501034,
0.00539687869229736,0.00552086330798511,0.00580159241745631,0.00598802814751206,
0.00629385847569466,0.00659968880387725,0.00684346074001378,0.00715186160191428,
0.00746782759000774,0.00769889333251549,0.00803469603381836,0.00837663399754488,
0.00855432592501721,0.0089155447774318,0.00917831546395288,0.00950363410224399,
0.00984133208955611,0.00993830453848906,0.0102651911100207,0.0107425161623785,
0.0112282340743661,0.0117224019296413,0.0119760562950241,0.0124966589117128,
0.0131154536646652,0.0136869214800275,0.0144195285788496,0.015146314613406,
0.0158818322443608,0.0166173498753156,0.0171086518500344,0.0176708895680441,
0.0177821681188111,0.0188947601276208,0.0189922862057886,0.0201663710327867,
0.0205303822200413,0.0215582587898393,0.0228151166104153,0.0239521125900482,
0.0243404099042828,0.0256629777750517,0.0265883729594407,0.0273738429600551),
 .UNSPECIFIED.);
#566=B_SPLINE_CURVE_WITH_KNOTS('',3,(#15300,#15301,#15302,#15303,#15304,
#15305,#15306,#15307,#15308,#15309,#15310,#15311,#15312,#15313,#15314,#15315,
#15316,#15317,#15318,#15319,#15320,#15321,#15322,#15323,#15324,#15325,#15326,
#15327,#15328,#15329,#15330,#15331,#15332,#15333,#15334,#15335,#15336,#15337,
#15338,#15339,#15340,#15341,#15342,#15343,#15344,#15345,#15346,#15347,#15348,
#15349,#15350,#15351,#15352,#15353,#15354,#15355,#15356,#15357,#15358,#15359,
#15360,#15361,#15362,#15363,#15364,#15365,#15366,#15367,#15368,#15369,#15370,
#15371,#15372,#15373,#15374,#15375,#15376,#15377,#15378,#15379,#15380,#15381,
#15382,#15383,#15384,#15385,#15386,#15387,#15388,#15389,#15390,#15391,#15392,
#15393,#15394,#15395,#15396,#15397,#15398,#15399,#15400,#15401,#15402,#15403,
#15404,#15405,#15406,#15407,#15408,#15409,#15410,#15411,#15412,#15413,#15414,
#15415,#15416,#15417,#15418,#15419,#15420,#15421,#15422,#15423,#15424,#15425,
#15426,#15427,#15428,#15429,#15430,#15431,#15432,#15433,#15434,#15435,#15436,
#15437,#15438,#15439,#15440,#15441,#15442,#15443,#15444,#15445,#15446,#15447,
#15448,#15449,#15450,#15451,#15452,#15453,#15454,#15455,#15456,#15457,#15458,
#15459,#15460,#15461,#15462,#15463,#15464,#15465,#15466,#15467,#15468,#15469,
#15470,#15471,#15472,#15473,#15474,#15475,#15476,#15477,#15478,#15479,#15480,
#15481,#15482,#15483,#15484,#15485,#15486,#15487,#15488,#15489,#15490,#15491,
#15492,#15493,#15494,#15495,#15496,#15497,#15498,#15499,#15500,#15501),
 .UNSPECIFIED.,.F.,.F.,(4,3,3,3,3,3,3,3,3,3,3,3,3,3,3,3,3,3,3,3,3,3,3,3,
3,3,3,3,3,3,3,3,3,3,3,3,3,3,3,3,3,3,3,3,3,3,3,3,3,3,3,3,3,3,3,3,3,3,3,3,
3,3,3,3,3,3,3,4),(-4.12191685327121E-5,0.00134365323327312,0.00266981737417628,
0.00298526322249882,0.0042758199183551,0.00549924207753177,0.00576110409467799,
0.0067865453003314,0.00795794545576501,0.00832117904489857,0.0094313041967944,
0.00952851739737183,0.0100894715329932,0.0102004275347635,0.0106906600420225,
0.0114215724738158,0.0121474549948729,0.0128808823820342,0.0136143097691955,
0.0142316850267863,0.0148018855520596,0.0153212508864116,0.0158152842107737,
0.0163008195651895,0.0165519989006371,0.0170281920036276,0.0173543633216557,
0.0176922781173,0.0180175516899865,0.0181126066147906,0.0184729983898973,
0.0187351331208436,0.0190770274958923,0.0194127390567275,0.0195886036794517,
0.0199052822990516,0.0202139762108961,0.0204420742380597,0.0206853098848451,
0.0209904273407564,0.0212955447966677,0.0215756224355253,0.0217616571699925,
0.0220253282929461,0.0221490153552757,0.0222660905809035,0.0225757506345797,
0.0227409940235605,0.0227526541063417,0.0229179562787235,0.0230024859138837,
0.0236631190939991,0.0238559564724917,0.0240349050279617,0.0242151179796911,
0.0242826917517957,0.024576223221583,0.0247094270310997,0.0247476705064236,
0.0250471595594179,0.0253085783382894,0.0255628975897077,0.0258781659521826,
0.025912261569786,0.0262516558540705,0.0265849804311658,0.0269274095690448,
0.0272698387069238),.UNSPECIFIED.);
#567=B_SPLINE_CURVE_WITH_KNOTS('',3,(#15503,#15504,#15505,#15506,#15507,
#15508,#15509,#15510,#15511,#15512,#15513,#15514,#15515,#15516,#15517,#15518,
#15519,#15520,#15521,#15522,#15523,#15524,#15525,#15526,#15527,#15528,#15529,
#15530,#15531,#15532,#15533,#15534,#15535,#15536,#15537,#15538,#15539,#15540,
#15541,#15542,#15543,#15544,#15545,#15546,#15547,#15548,#15549,#15550,#15551,
#15552,#15553,#15554,#15555,#15556,#15557,#15558,#15559,#15560,#15561,#15562,
#15563,#15564,#15565,#15566,#15567,#15568,#15569,#15570,#15571,#15572,#15573,
#15574,#15575,#15576,#15577,#15578,#15579,#15580,#15581,#15582,#15583,#15584,
#15585,#15586,#15587,#15588,#15589,#15590,#15591,#15592,#15593,#15594,#15595,
#15596,#15597,#15598,#15599),.UNSPECIFIED.,.F.,.F.,(4,3,3,3,3,3,3,3,3,3,
3,3,3,3,3,3,3,3,3,3,3,3,3,3,3,3,3,3,3,3,3,3,4),(0.,0.000237157711333885,
0.000465955627071617,0.000692471694688221,0.00101215149057648,0.00133755096760822,
0.00138494338937644,0.00154502472927642,0.00172378677637225,0.00190060093021846,
0.00207741508406466,0.00218381987505132,0.00244036367639352,0.00248194620057247,
0.00270340866436264,0.00276988677875289,0.00277353313349095,0.0030435391747074,
0.003116122626097,0.00324814486575857,0.00338255162160067,0.00346235847344111,
0.00364324318024271,0.00382965963813554,0.00399772979477703,0.00415483016812933,
0.00436117928878065,0.00457177672492627,0.0047886688078585,0.00484730186281755,
0.00507760552343842,0.00531594990564191,0.00553977355750578),
 .UNSPECIFIED.);
#568=B_SPLINE_CURVE_WITH_KNOTS('',3,(#15600,#15601,#15602,#15603,#15604,
#15605,#15606,#15607,#15608,#15609,#15610,#15611,#15612,#15613,#15614,#15615,
#15616,#15617,#15618,#15619,#15620,#15621,#15622,#15623,#15624,#15625,#15626,
#15627,#15628,#15629,#15630,#15631,#15632,#15633,#15634,#15635,#15636,#15637,
#15638,#15639,#15640,#15641,#15642,#15643,#15644,#15645,#15646,#15647,#15648,
#15649,#15650,#15651,#15652,#15653,#15654,#15655,#15656,#15657,#15658,#15659,
#15660,#15661,#15662,#15663,#15664,#15665,#15666,#15667,#15668,#15669,#15670,
#15671,#15672,#15673,#15674,#15675,#15676,#15677,#15678,#15679,#15680,#15681,
#15682,#15683,#15684,#15685,#15686,#15687,#15688,#15689,#15690,#15691,#15692,
#15693,#15694,#15695,#15696,#15697,#15698,#15699,#15700,#15701,#15702,#15703,
#15704,#15705,#15706,#15707,#15708,#15709,#15710,#15711,#15712,#15713,#15714,
#15715,#15716,#15717,#15718,#15719,#15720,#15721,#15722,#15723,#15724,#15725,
#15726,#15727,#15728,#15729,#15730,#15731,#15732,#15733,#15734,#15735,#15736,
#15737,#15738,#15739,#15740,#15741,#15742,#15743,#15744,#15745,#15746,#15747,
#15748,#15749,#15750,#15751,#15752,#15753,#15754,#15755,#15756,#15757,#15758,
#15759,#15760,#15761,#15762,#15763,#15764,#15765,#15766,#15767,#15768,#15769,
#15770,#15771,#15772,#15773,#15774,#15775,#15776,#15777,#15778,#15779,#15780,
#15781,#15782,#15783,#15784,#15785,#15786,#15787,#15788,#15789,#15790,#15791,
#15792,#15793,#15794,#15795,#15796,#15797,#15798,#15799,#15800,#15801),
 .UNSPECIFIED.,.F.,.F.,(4,3,3,3,3,3,3,3,3,3,3,3,3,3,3,3,3,3,3,3,3,3,3,3,
3,3,3,3,3,3,3,3,3,3,3,3,3,3,3,3,3,3,3,3,3,3,3,3,3,3,3,3,3,3,3,3,3,3,3,3,
3,3,3,3,3,3,3,4),(0.,0.000340175691736026,0.000675474341465466,0.00101808855420478,
0.0013607027669441,0.00167669716893931,0.0017108651850034,0.00196577589296195,
0.00226595430562214,0.00252797514522077,0.00256629777750511,0.00286050548518003,
0.00299401407375597,0.00317480367773506,0.00335423798419973,0.00342173037000683,
0.00408388793877329,0.00427716296250855,0.00444284813951406,0.00452758478188384,
0.00469321101548644,0.00470487925875941,0.00501526856889609,0.00513259555501027,
0.0053968786924259,0.00552086330798684,0.00580159241725754,0.00598802814751199,
0.00629385847569525,0.00659968880387851,0.00684346074001371,0.00715186160180756,
0.00746782758975846,0.00769889333251542,0.00803469603398907,0.00837663399785215,
0.00855432592501714,0.00891554477746769,0.00917831546395363,0.0095036341029607,
0.0098413320909301,0.00993830453849759,0.0102651911100206,0.010742516162387,
0.0112282340744698,0.0117224019298567,0.011976056295024,0.0124966589117161,
0.013115453665662,0.0136869214800275,0.0144195285788502,0.0151463146137948,
0.0158818322445567,0.0166173498753185,0.0171086518500343,0.017670889568476,
0.0177821681188137,0.0188947601244791,0.0189922862057895,0.0201663710329349,
0.0205303822200412,0.0215582587898413,0.0228151166108405,0.023952112590048,
0.0243404099042828,0.0256629777750514,0.0265883729179494,0.0273738429600549),
 .UNSPECIFIED.);
#569=B_SPLINE_CURVE_WITH_KNOTS('',3,(#15803,#15804,#15805,#15806,#15807,
#15808,#15809,#15810,#15811,#15812,#15813,#15814,#15815,#15816,#15817,#15818,
#15819,#15820,#15821,#15822,#15823,#15824,#15825,#15826,#15827,#15828,#15829,
#15830,#15831,#15832,#15833,#15834,#15835,#15836,#15837,#15838,#15839,#15840,
#15841,#15842,#15843,#15844,#15845,#15846,#15847,#15848,#15849,#15850,#15851,
#15852,#15853,#15854,#15855,#15856,#15857,#15858,#15859,#15860,#15861,#15862,
#15863,#15864,#15865,#15866,#15867,#15868,#15869,#15870,#15871,#15872,#15873,
#15874,#15875,#15876,#15877,#15878,#15879,#15880,#15881,#15882,#15883,#15884,
#15885,#15886,#15887,#15888,#15889,#15890,#15891,#15892,#15893,#15894,#15895,
#15896,#15897,#15898,#15899,#15900,#15901,#15902,#15903,#15904,#15905,#15906,
#15907,#15908,#15909,#15910,#15911,#15912,#15913,#15914,#15915,#15916,#15917,
#15918,#15919,#15920,#15921,#15922,#15923,#15924,#15925,#15926,#15927,#15928,
#15929,#15930,#15931,#15932,#15933,#15934,#15935,#15936,#15937,#15938,#15939,
#15940,#15941,#15942,#15943,#15944,#15945,#15946,#15947,#15948,#15949,#15950,
#15951,#15952,#15953,#15954,#15955,#15956,#15957,#15958,#15959,#15960,#15961,
#15962,#15963,#15964,#15965,#15966,#15967,#15968,#15969,#15970,#15971,#15972,
#15973,#15974,#15975,#15976,#15977,#15978,#15979,#15980,#15981,#15982,#15983,
#15984,#15985,#15986,#15987,#15988,#15989,#15990,#15991,#15992,#15993,#15994,
#15995,#15996,#15997,#15998,#15999,#16000,#16001,#16002,#16003,#16004),
 .UNSPECIFIED.,.F.,.F.,(4,3,3,3,3,3,3,3,3,3,3,3,3,3,3,3,3,3,3,3,3,3,3,3,
3,3,3,3,3,3,3,3,3,3,3,3,3,3,3,3,3,3,3,3,3,3,3,3,3,3,3,3,3,3,3,3,3,3,3,3,
3,3,3,3,3,3,3,4),(-4.12191685326785E-5,0.00134365322910891,0.00266981736923567,
0.0029852632224583,0.00427581991812639,0.00549924207859078,0.00576110409467375,
0.00678654530033131,0.00795794545614227,0.00832117904489245,0.00943130419171935,
0.00952851739736535,0.0100894715305543,0.0102004275347633,0.0106906600420251,
0.0114215724738176,0.0121474549939761,0.0128808823815857,0.0136143097691953,
0.0142316850264925,0.0148018855520585,0.0153212508864113,0.0158152842110432,
0.0163008195657759,0.0165519989006382,0.0170281920036273,0.0173543633216574,
0.0176922781166802,0.0180175516886633,0.0181126066147891,0.0184729983898273,
0.0187351331208433,0.0190770274957655,0.0194127390564447,0.0195886036794513,
0.0199052822991559,0.0202139762110683,0.0204420742380593,0.0206853098848451,
0.0209904273407562,0.0212955447966673,0.0215756224361278,0.0217616571699925,
0.0220253282935128,0.0221490153552753,0.0222660905809034,0.0225757506345793,
0.0227409940235518,0.0227526541063411,0.0229179562787035,0.0230024859138833,
0.0236631190935958,0.0238559564724913,0.0240349050279607,0.024215117979687,
0.0242826917517953,0.0245762232216197,0.0247094270310993,0.0247476705064231,
0.0250471595592009,0.0253085783382907,0.0255628975897073,0.0258781659535221,
0.0259122615697878,0.0262516558540717,0.0265849804309141,0.0269274095689187,
0.0272698387069233),.UNSPECIFIED.);
#570=B_SPLINE_CURVE_WITH_KNOTS('',3,(#16005,#16006,#16007,#16008,#16009,
#16010,#16011,#16012,#16013,#16014,#16015,#16016,#16017,#16018,#16019,#16020,
#16021,#16022,#16023,#16024,#16025,#16026,#16027,#16028,#16029,#16030,#16031,
#16032,#16033,#16034,#16035,#16036,#16037,#16038,#16039,#16040,#16041,#16042,
#16043,#16044,#16045,#16046,#16047,#16048,#16049,#16050,#16051,#16052,#16053),
 .UNSPECIFIED.,.F.,.F.,(4,3,3,3,3,3,3,3,3,3,3,3,3,3,3,3,4),(0.,0.000236842439941471,
0.000465418231564533,0.0006924716946882,0.00101111078066431,0.00133487521500561,
0.0013849433893764,0.00154319593245401,0.0017222487783158,0.0018998319311902,
0.0020774150840646,0.00228352041032069,0.00248574199847713,0.00268332977810061,
0.00276807256049863,0.0027698867787528,0.00277080264391651),
 .UNSPECIFIED.);
#571=B_SPLINE_CURVE_WITH_KNOTS('',3,(#16164,#16165,#16166,#16167,#16168,
#16169,#16170,#16171,#16172,#16173,#16174,#16175,#16176,#16177,#16178,#16179,
#16180,#16181,#16182,#16183,#16184,#16185,#16186,#16187),.UNSPECIFIED.,
 .F.,.F.,(4,2,2,2,2,2,2,2,2,2,2,4),(0.,0.000297119359731175,0.00059423871946235,
0.0011884774389247,0.0023769548778494,0.00475390975569881,0.00713086463354823,
0.00950781951139764,0.0142617292670965,0.0166386841449459,0.0178271615838706,
0.0190156390227953),.UNSPECIFIED.);
#572=B_SPLINE_CURVE_WITH_KNOTS('',3,(#16342,#16343,#16344,#16345,#16346,
#16347,#16348,#16349,#16350,#16351,#16352,#16353,#16354,#16355,#16356,#16357,
#16358,#16359,#16360,#16361),.UNSPECIFIED.,.F.,.F.,(4,2,2,2,2,2,2,2,2,4),
(-4.50312400614093E-5,0.00472460449543289,0.00949424023092719,0.0118790580986743,
0.0142638759664215,0.0166486938341686,0.0178411027680422,0.018437307234979,
0.0187354094684474,0.0190335117019158),.UNSPECIFIED.);
#573=B_SPLINE_CURVE_WITH_KNOTS('',3,(#16471,#16472,#16473,#16474,#16475,
#16476,#16477,#16478,#16479,#16480,#16481,#16482,#16483,#16484,#16485,#16486,
#16487,#16488,#16489,#16490),.UNSPECIFIED.,.F.,.F.,(4,2,2,2,2,2,2,2,2,4),
(-4.50312400612699E-5,0.00472460449542813,0.00949424023091753,0.0118790580986622,
0.0142638759664069,0.0166486938341516,0.017841102768024,0.0184373072349602,
0.0187354094684283,0.0190335117018964),.UNSPECIFIED.);
#574=B_SPLINE_CURVE_WITH_KNOTS('',3,(#16646,#16647,#16648,#16649,#16650,
#16651,#16652,#16653,#16654,#16655,#16656,#16657,#16658,#16659,#16660,#16661,
#16662,#16663,#16664,#16665,#16666,#16667,#16668,#16669),.UNSPECIFIED.,
 .F.,.F.,(4,2,2,2,2,2,2,2,2,2,2,4),(8.56187529156079E-17,0.000297119359731277,
0.000594238719462469,0.00118847743892484,0.00237695487784958,0.00475390975569906,
0.00713086463354855,0.00950781951139803,0.014261729267097,0.0166386841449465,
0.0178271615838712,0.019015639022796),.UNSPECIFIED.);
#575=B_SPLINE_CURVE_WITH_KNOTS('',3,(#17026,#17027,#17028,#17029,#17030,
#17031,#17032,#17033,#17034,#17035,#17036,#17037,#17038,#17039,#17040,#17041,
#17042,#17043,#17044,#17045,#17046,#17047,#17048,#17049,#17050,#17051,#17052,
#17053),.UNSPECIFIED.,.F.,.F.,(4,3,3,3,3,3,3,3,3,4),(0.,0.000231294325945477,
0.000464822662229606,0.000605683234682749,0.000808855738910866,0.0010118571627786,
0.0012113664693655,0.00144599958458062,0.00168128722210177,0.0018161530161823),
 .UNSPECIFIED.);
#576=B_SPLINE_CURVE_WITH_KNOTS('',3,(#17054,#17055,#17056,#17057,#17058,
#17059,#17060,#17061,#17062,#17063,#17064,#17065,#17066,#17067,#17068,#17069,
#17070,#17071,#17072,#17073,#17074,#17075,#17076,#17077,#17078,#17079,#17080,
#17081,#17082,#17083,#17084,#17085,#17086,#17087,#17088,#17089,#17090,#17091,
#17092,#17093,#17094,#17095,#17096,#17097,#17098,#17099,#17100,#17101,#17102,
#17103,#17104,#17105,#17106,#17107,#17108,#17109,#17110,#17111,#17112,#17113,
#17114,#17115,#17116,#17117,#17118,#17119,#17120,#17121,#17122,#17123,#17124,
#17125,#17126,#17127,#17128,#17129,#17130,#17131,#17132,#17133,#17134,#17135,
#17136,#17137,#17138,#17139,#17140,#17141,#17142,#17143,#17144,#17145,#17146,
#17147,#17148,#17149,#17150,#17151,#17152,#17153,#17154,#17155,#17156,#17157,
#17158,#17159,#17160,#17161,#17162,#17163,#17164,#17165,#17166,#17167,#17168,
#17169,#17170,#17171,#17172,#17173,#17174,#17175,#17176,#17177,#17178,#17179,
#17180,#17181,#17182,#17183,#17184,#17185,#17186,#17187,#17188,#17189,#17190,
#17191,#17192,#17193,#17194,#17195,#17196,#17197,#17198,#17199,#17200,#17201,
#17202,#17203,#17204,#17205,#17206,#17207,#17208,#17209,#17210,#17211,#17212,
#17213,#17214,#17215,#17216,#17217,#17218,#17219,#17220,#17221,#17222,#17223,
#17224,#17225,#17226,#17227,#17228,#17229,#17230,#17231,#17232,#17233,#17234,
#17235,#17236,#17237,#17238,#17239,#17240,#17241,#17242,#17243,#17244,#17245,
#17246,#17247,#17248,#17249,#17250,#17251,#17252,#17253,#17254,#17255,#17256,
#17257,#17258,#17259,#17260,#17261,#17262,#17263,#17264,#17265,#17266,#17267,
#17268,#17269,#17270,#17271,#17272,#17273,#17274,#17275,#17276,#17277,#17278,
#17279,#17280,#17281,#17282,#17283,#17284,#17285,#17286,#17287,#17288,#17289,
#17290,#17291,#17292,#17293,#17294,#17295,#17296,#17297,#17298,#17299,#17300,
#17301,#17302,#17303,#17304,#17305,#17306,#17307,#17308,#17309,#17310,#17311,
#17312,#17313,#17314,#17315,#17316,#17317,#17318,#17319,#17320,#17321,#17322,
#17323,#17324),.UNSPECIFIED.,.F.,.F.,(4,3,3,3,3,3,3,3,3,3,3,3,3,3,3,3,3,
3,3,3,3,3,3,3,3,3,3,3,3,3,3,3,3,3,3,3,3,3,3,3,3,3,3,3,3,3,3,3,3,3,3,3,3,
3,3,3,3,3,3,3,3,3,3,3,3,3,3,3,3,3,3,3,3,3,3,3,3,3,3,3,3,3,3,3,3,3,3,3,3,
3,4),(0.0018161530161823,0.00181704970404825,0.00200583370208725,0.00219446082802312,
0.00238336003013788,0.00242273293873099,0.00265759191053558,0.00289143223371987,
0.00302841617341374,0.00327576515313478,0.00352338277376447,0.00363409940809649,
0.00391111582115793,0.00418763440557408,0.00423978264277924,0.00447293482787131,
0.00470764138266438,0.00484546587746199,0.00503561213322781,0.00522552979015431,
0.00541560630890245,0.00545114911214474,0.00568628229470434,0.00592131468169729,
0.00605683234682749,0.00625531156903434,0.00645891357527229,0.00666251558151024,
0.00689644101753518,0.00712864478231464,0.00726819881619298,0.00752881290938141,
0.00779301232002778,0.00787388205087573,0.00808290763071909,0.00829174641109551,
0.00847956528555848,0.00871398900637753,0.00894924091999715,0.00908524852024123,
0.00927328004700098,0.00946113685411365,0.0096492486498554,0.00969093175492398,
0.00992591903218147,0.0101600600236151,0.0102966149896067,0.0105267869044746,
0.0107572068987285,0.0109022982242895,0.0112461276330547,0.0115079814589722,
0.0117407454265451,0.0119752296007021,0.012113664693655,0.0123056711978274,
0.0124974413983672,0.0126893421942621,0.0127193479283377,0.0129544208220635,
0.0131895714004269,0.0133250311630205,0.0135200587949984,0.0137150013702892,
0.0139102531895133,0.0139307143977032,0.0141649164284798,0.0143975585284212,
0.014536397632386,0.0148611323777672,0.0151420808670687,0.0153588623255755,
0.0155754441480225,0.0157477641017515,0.0159819424694056,0.0162171239137906,
0.0163534473364342,0.0165412047623366,0.0167287716064859,0.0169165741256843,
0.016959130571117,0.017194210781073,0.0174286191974533,0.0175648138057997,
0.0177834673516284,0.0180023569372318,0.0181704970404825,0.0184733386578238,
0.0187705466100904,0.0190762050599692,0.019381863509848),.UNSPECIFIED.);
#577=B_SPLINE_CURVE_WITH_KNOTS('',3,(#17327,#17328,#17329,#17330,#17331,
#17332,#17333,#17334,#17335,#17336,#17337,#17338,#17339,#17340,#17341,#17342,
#17343,#17344,#17345,#17346,#17347,#17348,#17349,#17350,#17351,#17352,#17353,
#17354,#17355,#17356,#17357,#17358,#17359,#17360,#17361,#17362,#17363,#17364,
#17365,#17366,#17367,#17368,#17369,#17370,#17371,#17372,#17373,#17374,#17375,
#17376,#17377,#17378,#17379,#17380,#17381,#17382,#17383,#17384,#17385,#17386,
#17387,#17388,#17389,#17390,#17391,#17392,#17393,#17394,#17395,#17396,#17397,
#17398,#17399,#17400,#17401,#17402,#17403,#17404,#17405,#17406,#17407,#17408,
#17409,#17410,#17411,#17412,#17413,#17414,#17415,#17416,#17417,#17418,#17419,
#17420,#17421,#17422,#17423,#17424,#17425,#17426,#17427,#17428,#17429,#17430,
#17431,#17432,#17433,#17434,#17435,#17436,#17437,#17438,#17439,#17440,#17441,
#17442,#17443,#17444,#17445,#17446,#17447,#17448,#17449,#17450,#17451,#17452,
#17453,#17454,#17455,#17456,#17457,#17458,#17459,#17460,#17461,#17462,#17463,
#17464,#17465,#17466,#17467,#17468,#17469,#17470,#17471,#17472,#17473,#17474,
#17475,#17476,#17477,#17478,#17479,#17480,#17481,#17482,#17483,#17484,#17485,
#17486,#17487,#17488,#17489,#17490,#17491,#17492,#17493,#17494,#17495,#17496,
#17497,#17498,#17499,#17500,#17501,#17502,#17503,#17504,#17505,#17506,#17507,
#17508,#17509,#17510,#17511,#17512,#17513,#17514,#17515,#17516,#17517,#17518,
#17519,#17520,#17521,#17522,#17523,#17524,#17525,#17526,#17527,#17528,#17529,
#17530,#17531,#17532,#17533,#17534,#17535,#17536,#17537,#17538,#17539,#17540,
#17541,#17542,#17543,#17544,#17545,#17546,#17547,#17548,#17549,#17550,#17551,
#17552,#17553,#17554,#17555,#17556,#17557,#17558,#17559,#17560,#17561,#17562,
#17563,#17564,#17565,#17566,#17567,#17568,#17569,#17570,#17571,#17572,#17573,
#17574,#17575,#17576,#17577,#17578,#17579,#17580,#17581,#17582,#17583,#17584,
#17585,#17586,#17587,#17588,#17589,#17590,#17591,#17592,#17593,#17594,#17595,
#17596,#17597,#17598,#17599,#17600,#17601,#17602,#17603),.UNSPECIFIED.,
 .F.,.F.,(4,3,3,3,3,3,3,3,3,3,3,3,3,3,3,3,3,3,3,3,3,3,3,3,3,3,3,3,3,3,3,
3,3,3,3,3,3,3,3,3,3,3,3,3,3,3,3,3,3,3,3,3,3,3,3,3,3,3,3,3,3,3,3,3,3,3,3,
3,3,3,3,3,3,3,3,3,3,3,3,3,3,3,3,3,3,3,3,3,3,3,3,3,4),(0.,0.000231293909478829,
0.000464821929767556,0.00060568320508766,0.000808857863905471,0.00101186144647658,
0.00121136641017532,0.00144600104230718,0.00168128763074085,0.00181704961526298,
0.00200583317153906,0.00219445983447999,0.00238335854916359,0.00242273282035064,
0.00265759194929965,0.00289143243005884,0.0030284160254383,0.003275743635374,
0.00352333983374325,0.00363409923052596,0.00391114756596992,0.00418769750088776,
0.00423978243561362,0.00447293416717338,0.00470764050251022,0.00484546564070128,
0.00503561332151353,0.00522553241631793,0.00541561037723325,0.00545114884578894,
0.0056862816780372,0.00592131384823276,0.0060568320508766,0.00625531070847705,
0.00645891298222066,0.00666251525596426,0.00689644055875581,0.00712864418863787,
0.00726819846105192,0.00752884048815537,0.00779306949700858,0.00787388166613958,
0.00808291222402555,0.00829175595352107,0.00847956487122724,0.00871398849583979,
0.00894924051298378,0.0090852480763149,0.00927327916167684,0.00946113552646327,
0.0096492468822708,0.00969093128140256,0.00992591855977248,0.0101600597593885,
0.0102966144864902,0.0105267831616192,0.0107571999178322,0.0109022976915779,
0.0112461788451932,0.0115079808966655,0.0117407448529832,0.0119752289995473,
0.0121136641017532,0.0123056716422985,0.0124974428571561,0.0126893446268732,
0.0127193473068409,0.0129544204495954,0.0131895713760254,0.0133250305119285,
0.0135200544620049,0.0137149933329001,0.0139102414502059,0.0139307137170162,
0.0141649161753979,0.0143975589201434,0.0145363969221038,0.0148611855057929,
0.0151420801271915,0.0153588661585815,0.0155754525660823,0.0157477633322792,
0.0159819413893676,0.0162171225409267,0.0163534465373668,0.0165412039988469,
0.016728770858437,0.0169165733652975,0.0169591297424545,0.0171942100555913,
0.0174286185839122,0.0175648129475421,0.0175712098172771),.UNSPECIFIED.);
#578=B_SPLINE_CURVE_WITH_KNOTS('',3,(#17604,#17605,#17606,#17607,#17608,
#17609,#17610,#17611,#17612,#17613,#17614,#17615,#17616,#17617,#17618,#17619,
#17620,#17621,#17622,#17623,#17624,#17625),.UNSPECIFIED.,.F.,.F.,(4,3,3,
3,3,3,3,4),(0.0175712098172771,0.0177898520948126,0.0180087321653697,0.0181704961526298,
0.0184733377551736,0.0187705437287487,0.0190762031457769,0.0193818625628051),
 .UNSPECIFIED.);
#579=B_SPLINE_CURVE_WITH_KNOTS('',3,(#18006,#18007,#18008,#18009,#18010,
#18011,#18012,#18013,#18014,#18015,#18016,#18017,#18018,#18019,#18020,#18021,
#18022,#18023),.UNSPECIFIED.,.F.,.F.,(4,2,2,2,2,2,2,2,4),(0.866318752317526,
0.974859456130365,1.08340015994321,1.19143914420975,1.29947812847629,1.40751711274283,
1.51555609700937,1.62409680082221,1.73263750463505),.UNSPECIFIED.);
#580=B_SPLINE_CURVE_WITH_KNOTS('',3,(#18024,#18025,#18026,#18027,#18028,
#18029,#18030,#18031,#18032,#18033,#18034,#18035,#18036,#18037,#18038,#18039,
#18040,#18041),.UNSPECIFIED.,.F.,.F.,(4,2,2,2,2,2,2,2,4),(1.73263750463505,
1.84117820844789,1.94971891226073,2.05775789652727,2.16579688079381,2.27383586506035,
2.3818748493269,2.49041555313974,2.59895625695258),.UNSPECIFIED.);
#581=B_SPLINE_CURVE_WITH_KNOTS('',3,(#21100,#21101,#21102,#21103,#21104,
#21105,#21106,#21107,#21108,#21109,#21110,#21111,#21112,#21113,#21114,#21115,
#21116,#21117),.UNSPECIFIED.,.F.,.F.,(4,2,2,2,2,2,2,2,4),(0.,0.0591297066253043,
0.101286062949422,0.137517711401243,0.179810134914136,0.212974667045344,
0.229441128614405,0.242688203236853,0.242937404635999),.UNSPECIFIED.);
#582=B_SPLINE_CURVE_WITH_KNOTS('',3,(#21121,#21122,#21123,#21124,#21125,
#21126,#21127,#21128,#21129,#21130,#21131,#21132,#21133,#21134,#21135,#21136),
 .UNSPECIFIED.,.F.,.F.,(4,2,2,2,2,2,2,4),(0.242619551178519,0.255524854267213,
0.271696804230175,0.303396718536254,0.343221718357041,0.379813718288485,
0.420371936847968,0.486941959854264),.UNSPECIFIED.);
#583=B_SPLINE_CURVE_WITH_KNOTS('',3,(#21141,#21142,#21143,#21144,#21145,
#21146,#21147,#21148,#21149,#21150,#21151,#21152,#21153,#21154,#21155,#21156,
#21157,#21158),.UNSPECIFIED.,.F.,.F.,(4,2,2,2,2,2,2,2,4),(0.,0.0625576155549603,
0.103705894629019,0.140114223826818,0.180905683903664,0.212584741865507,
0.229068999283201,0.242305782037659,0.242619551178519),.UNSPECIFIED.);
#584=B_SPLINE_CURVE_WITH_KNOTS('',3,(#21161,#21162,#21163,#21164,#21165,
#21166,#21167,#21168,#21169,#21170,#21171,#21172,#21173,#21174,#21175,#21176),
 .UNSPECIFIED.,.F.,.F.,(4,2,2,2,2,2,2,4),(0.242937404635999,0.255921391403813,
0.272139917047041,0.304029069944799,0.344156916496348,0.380728183501685,
0.421482205148501,0.485707929360947),.UNSPECIFIED.);
#585=B_SPLINE_CURVE_WITH_KNOTS('',3,(#21179,#21180,#21181,#21182,#21183,
#21184,#21185,#21186,#21187,#21188,#21189,#21190,#21191,#21192,#21193,#21194,
#21195,#21196,#21197,#21198,#21199,#21200,#21201,#21202,#21203,#21204,#21205,
#21206,#21207,#21208),.UNSPECIFIED.,.F.,.F.,(4,2,2,2,2,2,2,2,2,2,2,2,2,
2,4),(0.,0.0591297066251443,0.10128606294921,0.137517711400911,0.179810134913968,
0.212974667045338,0.22944112861441,0.242688203236827,0.255921391403934,
0.272139917047388,0.304029069945497,0.3441569164974,0.380728183503124,0.421482205150273,
0.485707929363829),.UNSPECIFIED.);
#586=B_SPLINE_CURVE_WITH_KNOTS('',3,(#21212,#21213,#21214,#21215,#21216,
#21217,#21218,#21219,#21220,#21221,#21222,#21223,#21224,#21225,#21226,#21227,
#21228,#21229,#21230,#21231,#21232,#21233,#21234,#21235,#21236,#21237,#21238,
#21239,#21240,#21241),.UNSPECIFIED.,.F.,.F.,(4,2,2,2,2,2,2,2,2,2,2,2,2,
2,4),(0.,0.0625576155550425,0.103705894629037,0.140114223826745,0.180905683903574,
0.212584741865456,0.229068999283225,0.242305782037766,0.255524854267145,
0.271696804229871,0.303396718535534,0.343221718355779,0.379813718286607,
0.420371936845398,0.486941959850739),.UNSPECIFIED.);
#587=B_SPLINE_CURVE_WITH_KNOTS('',3,(#21245,#21246,#21247,#21248,#21249,
#21250,#21251,#21252,#21253,#21254,#21255,#21256,#21257,#21258,#21259,#21260,
#21261,#21262,#21263,#21264,#21265,#21266,#21267,#21268,#21269,#21270,#21271,
#21272,#21273,#21274),.UNSPECIFIED.,.F.,.F.,(4,2,2,2,2,2,2,2,2,2,2,2,2,
2,4),(0.,0.0591297066252864,0.101286062949393,0.137517711401177,0.179810134914117,
0.212974667045378,0.229441128614418,0.242688203236773,0.255921391403745,
0.272139917047061,0.304029069945025,0.344156916496804,0.380728183502349,
0.421482205149371,0.48570792936228),.UNSPECIFIED.);
#588=B_SPLINE_CURVE_WITH_KNOTS('',3,(#21278,#21279,#21280,#21281,#21282,
#21283,#21284,#21285,#21286,#21287,#21288,#21289,#21290,#21291,#21292,#21293,
#21294,#21295,#21296,#21297,#21298,#21299,#21300,#21301,#21302,#21303,#21304,
#21305,#21306,#21307),.UNSPECIFIED.,.F.,.F.,(4,2,2,2,2,2,2,2,2,2,2,2,2,
2,4),(0.,0.0625576155549716,0.103705894629009,0.140114223826776,0.180905683903617,
0.212584741865472,0.22906899928318,0.242305782037708,0.255524854267209,
0.271696804230295,0.303396718536698,0.343221718357867,0.379813718289666,
0.420371936849526,0.486941959856497),.UNSPECIFIED.);
#589=B_SPLINE_CURVE_WITH_KNOTS('',3,(#21311,#21312,#21313,#21314,#21315,
#21316,#21317,#21318,#21319,#21320,#21321,#21322,#21323,#21324,#21325,#21326,
#21327,#21328,#21329,#21330,#21331,#21332,#21333,#21334,#21335,#21336,#21337,
#21338,#21339,#21340),.UNSPECIFIED.,.F.,.F.,(4,2,2,2,2,2,2,2,2,2,2,2,2,
2,4),(0.,0.0591297066254632,0.101286062949567,0.137517711401381,0.179810134914222,
0.212974667045435,0.229441128614477,0.242688203236797,0.255921391403683,
0.272139917046899,0.304029069944637,0.344156916496141,0.380728183501339,
0.421482205148018,0.485707929360225),.UNSPECIFIED.);
#590=B_SPLINE_CURVE_WITH_KNOTS('',3,(#21344,#21345,#21346,#21347,#21348,
#21349,#21350,#21351,#21352,#21353,#21354,#21355,#21356,#21357,#21358,#21359,
#21360,#21361,#21362,#21363,#21364,#21365,#21366,#21367,#21368,#21369,#21370,
#21371,#21372,#21373),.UNSPECIFIED.,.F.,.F.,(4,2,2,2,2,2,2,2,2,2,2,2,2,
2,4),(0.,0.0625576155549251,0.103705894629016,0.140114223826815,0.180905683903673,
0.212584741865495,0.229068999283176,0.242305782037738,0.255524854267565,
0.271696804230953,0.303396718537859,0.343221718359601,0.379813718291938,
0.420371936852435,0.486941959860366),.UNSPECIFIED.);
#591=B_SPLINE_CURVE_WITH_KNOTS('',3,(#21377,#21378,#21379,#21380,#21381,
#21382,#21383,#21384,#21385,#21386,#21387,#21388,#21389,#21390,#21391,#21392,
#21393,#21394,#21395,#21396,#21397,#21398,#21399,#21400,#21401,#21402,#21403,
#21404,#21405,#21406),.UNSPECIFIED.,.F.,.F.,(4,2,2,2,2,2,2,2,2,2,2,2,2,
2,4),(0.,0.0591297066254656,0.101286062949478,0.137517711401217,0.179810134914112,
0.212974667045368,0.229441128614476,0.242688203236961,0.255921391404029,
0.272139917047424,0.30402906994545,0.344156916497263,0.38072818350272,0.421482205149666,
0.485707929362617),.UNSPECIFIED.);
#592=B_SPLINE_CURVE_WITH_KNOTS('',3,(#21410,#21411,#21412,#21413,#21414,
#21415,#21416,#21417,#21418,#21419,#21420,#21421,#21422,#21423,#21424,#21425,
#21426,#21427,#21428,#21429,#21430,#21431,#21432,#21433,#21434,#21435,#21436,
#21437,#21438,#21439),.UNSPECIFIED.,.F.,.F.,(4,2,2,2,2,2,2,2,2,2,2,2,2,
2,4),(0.,0.0625576155549631,0.103705894628963,0.140114223826657,0.18090568390353,
0.212584741865409,0.229068999283161,0.242305782037703,0.255524854267285,
0.271696804230179,0.303396718536041,0.343221718356524,0.379813718287668,
0.420371936846778,0.486941959852788),.UNSPECIFIED.);
#593=B_SPLINE_CURVE_WITH_KNOTS('',3,(#21443,#21444,#21445,#21446,#21447,
#21448,#21449,#21450,#21451,#21452,#21453,#21454,#21455,#21456,#21457,#21458,
#21459,#21460,#21461,#21462,#21463,#21464,#21465,#21466,#21467,#21468,#21469,
#21470,#21471,#21472),.UNSPECIFIED.,.F.,.F.,(4,2,2,2,2,2,2,2,2,2,2,2,2,
2,4),(0.,0.059129706625303,0.101286062949409,0.137517711401222,0.179810134914118,
0.212974667045327,0.229441128614365,0.242688203236767,0.255921391403782,
0.272139917047142,0.304029069945151,0.344156916497017,0.38072818350263,
0.421482205149739,0.48570792936266),.UNSPECIFIED.);
#594=B_SPLINE_CURVE_WITH_KNOTS('',3,(#21476,#21477,#21478,#21479,#21480,
#21481,#21482,#21483,#21484,#21485,#21486,#21487,#21488,#21489,#21490,#21491,
#21492,#21493,#21494,#21495,#21496,#21497,#21498,#21499,#21500,#21501,#21502,
#21503,#21504,#21505),.UNSPECIFIED.,.F.,.F.,(4,2,2,2,2,2,2,2,2,2,2,2,2,
2,4),(0.,0.0625576155549589,0.103705894629042,0.140114223826835,0.180905683903654,
0.212584741865466,0.229068999283114,0.242305782037558,0.255524854267162,
0.271696804230271,0.303396718536633,0.34322171835775,0.379813718289504,
0.420371936849334,0.486941959856202),.UNSPECIFIED.);
#595=B_SPLINE_CURVE_WITH_KNOTS('',3,(#21509,#21510,#21511,#21512,#21513,
#21514,#21515,#21516,#21517,#21518,#21519,#21520,#21521,#21522,#21523,#21524,
#21525,#21526,#21527,#21528,#21529,#21530,#21531,#21532,#21533,#21534,#21535,
#21536,#21537,#21538),.UNSPECIFIED.,.F.,.F.,(4,2,2,2,2,2,2,2,2,2,2,2,2,
2,4),(0.,0.0591297066253938,0.101286062949474,0.137517711401263,0.179810134914156,
0.212974667045388,0.229441128614457,0.242688203236794,0.255921391403719,
0.272139917047063,0.304029069945052,0.344156916496837,0.380728183502336,
0.421482205149336,0.485707929362192),.UNSPECIFIED.);
#596=B_SPLINE_CURVE_WITH_KNOTS('',3,(#21542,#21543,#21544,#21545,#21546,
#21547,#21548,#21549,#21550,#21551,#21552,#21553,#21554,#21555,#21556,#21557,
#21558,#21559,#21560,#21561,#21562,#21563,#21564,#21565,#21566,#21567,#21568,
#21569,#21570,#21571),.UNSPECIFIED.,.F.,.F.,(4,2,2,2,2,2,2,2,2,2,2,2,2,
2,4),(0.,0.0625576155548974,0.103705894628924,0.140114223826715,0.180905683903631,
0.212584741865498,0.229068999283233,0.242305782037817,0.255524854267415,
0.271696804230564,0.303396718537098,0.343221718358438,0.379813718290417,
0.420371936850418,0.486941959857704),.UNSPECIFIED.);
#597=B_SPLINE_CURVE_WITH_KNOTS('',3,(#21575,#21576,#21577,#21578,#21579,
#21580,#21581,#21582,#21583,#21584,#21585,#21586,#21587,#21588,#21589,#21590,
#21591,#21592,#21593,#21594,#21595,#21596,#21597,#21598,#21599,#21600,#21601,
#21602,#21603,#21604),.UNSPECIFIED.,.F.,.F.,(4,2,2,2,2,2,2,2,2,2,2,2,2,
2,4),(0.,0.0591297066250036,0.101286062949091,0.137517711400804,0.179810134913944,
0.21297466704533,0.229441128614477,0.242688203236995,0.255921391404044,
0.272139917047368,0.304029069945175,0.344156916496678,0.380728183502119,
0.421482205148957,0.485707929362086),.UNSPECIFIED.);
#598=B_SPLINE_CURVE_WITH_KNOTS('',3,(#21608,#21609,#21610,#21611,#21612,
#21613,#21614,#21615,#21616,#21617,#21618,#21619,#21620,#21621,#21622,#21623,
#21624,#21625,#21626,#21627,#21628,#21629,#21630,#21631,#21632,#21633,#21634,
#21635,#21636,#21637),.UNSPECIFIED.,.F.,.F.,(4,2,2,2,2,2,2,2,2,2,2,2,2,
2,4),(0.,0.0625576155550406,0.103705894629032,0.140114223826711,0.18090568390349,
0.21258474186536,0.229068999283064,0.242305782037584,0.255524854267104,
0.271696804230055,0.303396718536132,0.343221718356878,0.379813718288151,
0.420371936847442,0.486941959853629),.UNSPECIFIED.);
#599=B_SPLINE_CURVE_WITH_KNOTS('',3,(#21641,#21642,#21643,#21644,#21645,
#21646,#21647,#21648,#21649,#21650,#21651,#21652,#21653,#21654,#21655,#21656,
#21657,#21658,#21659,#21660,#21661,#21662,#21663,#21664,#21665,#21666,#21667,
#21668,#21669,#21670),.UNSPECIFIED.,.F.,.F.,(4,2,2,2,2,2,2,2,2,2,2,2,2,
2,4),(0.,0.0591297066253794,0.10128606294941,0.137517711401119,0.179810134914014,
0.212974667045288,0.229441128614387,0.242688203236939,0.255921391404106,
0.272139917047586,0.304029069945836,0.344156916497933,0.380728183503669,
0.421482205150903,0.485707929364375),.UNSPECIFIED.);
#600=B_SPLINE_CURVE_WITH_KNOTS('',3,(#21674,#21675,#21676,#21677,#21678,
#21679,#21680,#21681,#21682,#21683,#21684,#21685,#21686,#21687,#21688,#21689,
#21690,#21691,#21692,#21693,#21694,#21695,#21696,#21697,#21698,#21699,#21700,
#21701,#21702,#21703),.UNSPECIFIED.,.F.,.F.,(4,2,2,2,2,2,2,2,2,2,2,2,2,
2,4),(0.,0.062557615554957,0.103705894628953,0.140114223826674,0.180905683903591,
0.212584741865488,0.229068999283227,0.242305782037741,0.255524854267291,
0.271696804230317,0.303396718536427,0.3432217183572,0.379813718288632,0.420371936848053,
0.486941959854542),.UNSPECIFIED.);
#601=B_SPLINE_CURVE_WITH_KNOTS('',3,(#21707,#21708,#21709,#21710,#21711,
#21712,#21713,#21714,#21715,#21716,#21717,#21718,#21719,#21720,#21721,#21722,
#21723,#21724,#21725,#21726,#21727,#21728,#21729,#21730,#21731,#21732,#21733,
#21734,#21735,#21736),.UNSPECIFIED.,.F.,.F.,(4,2,2,2,2,2,2,2,2,2,2,2,2,
2,4),(0.,0.0591297066254563,0.101286062949547,0.137517711401359,0.179810134914195,
0.212974667045375,0.229441128614446,0.24268820323693,0.255921391404018,
0.272139917047466,0.304029069945651,0.34415691649772,0.380728183503433,
0.421482205150684,0.485707929363767),.UNSPECIFIED.);
#602=B_SPLINE_CURVE_WITH_KNOTS('',3,(#21740,#21741,#21742,#21743,#21744,
#21745,#21746,#21747,#21748,#21749,#21750,#21751,#21752,#21753,#21754,#21755,
#21756,#21757,#21758,#21759,#21760,#21761,#21762,#21763,#21764,#21765,#21766,
#21767,#21768,#21769),.UNSPECIFIED.,.F.,.F.,(4,2,2,2,2,2,2,2,2,2,2,2,2,
2,4),(0.,0.0625576155549561,0.103705894629025,0.140114223826833,0.18090568390366,
0.212584741865487,0.229068999283183,0.242305782037646,0.25552485426716,
0.271696804230063,0.303396718535982,0.343221718356607,0.379813718287887,
0.420371936847143,0.486941959853062),.UNSPECIFIED.);
#603=B_SPLINE_CURVE_WITH_KNOTS('',3,(#21777,#21778,#21779,#21780,#21781,
#21782,#21783,#21784,#21785,#21786),.UNSPECIFIED.,.F.,.F.,(4,2,2,2,4),(-0.46979780856301,
-0.352361341367453,-0.234924874171897,-0.117462437085949,0.),
 .UNSPECIFIED.);
#604=B_SPLINE_CURVE_WITH_KNOTS('',3,(#21788,#21789,#21790,#21791,#21792,
#21793,#21794,#21795,#21796,#21797),.UNSPECIFIED.,.F.,.F.,(4,2,2,2,4),(0.,
0.117462437085949,0.234924874171897,0.352361341367453,0.46979780856301),
 .UNSPECIFIED.);
#605=B_SPLINE_CURVE_WITH_KNOTS('',3,(#21802,#21803,#21804,#21805,#21806,
#21807,#21808,#21809,#21810,#21811),.UNSPECIFIED.,.F.,.F.,(4,2,2,2,4),(0.46979780856301,
0.587234275758566,0.704670742954122,0.822133180040071,0.939595617126019),
 .UNSPECIFIED.);
#606=B_SPLINE_CURVE_WITH_KNOTS('',3,(#21812,#21813,#21814,#21815,#21816,
#21817,#21818,#21819,#21820,#21821),.UNSPECIFIED.,.F.,.F.,(4,2,2,2,4),(-0.939595617126019,
-0.822133180040071,-0.704670742954122,-0.587234275758566,-0.46979780856301),
 .UNSPECIFIED.);
#607=B_SPLINE_CURVE_WITH_KNOTS('',3,(#21824,#21825,#21826,#21827,#21828,
#21829,#21830,#21831,#21832,#21833),.UNSPECIFIED.,.F.,.F.,(4,2,2,2,4),(-0.46979780856301,
-0.352361341367453,-0.234924874171897,-0.117462437085949,0.),
 .UNSPECIFIED.);
#608=B_SPLINE_CURVE_WITH_KNOTS('',3,(#21834,#21835,#21836,#21837,#21838,
#21839,#21840,#21841,#21842,#21843,#21844,#21845,#21846,#21847,#21848,#21849,
#21850,#21851,#21852,#21853,#21854,#21855,#21856,#21857,#21858,#21859),
 .UNSPECIFIED.,.F.,.F.,(4,2,2,2,2,2,2,2,2,2,2,2,4),(0.,0.117462437085949,
0.234924874171897,0.352361341367453,0.46979780856301,0.587234275758566,
0.704670742954122,0.822133180040071,0.939595617126019,1.05705805421197,
1.17452049129792,1.29195695849347,1.40939342568903),.UNSPECIFIED.);
#609=B_SPLINE_CURVE_WITH_KNOTS('',3,(#21868,#21869,#21870,#21871,#21872,
#21873,#21874,#21875,#21876,#21877,#21878,#21879,#21880,#21881,#21882,#21883,
#21884,#21885,#21886,#21887,#21888,#21889,#21890),.UNSPECIFIED.,.F.,.F.,
(4,2,2,2,3,2,2,2,2,2,4),(-0.353056606424783,-0.270966220923752,-0.175803528294806,
-0.0859129119745955,0.,0.0556570980636411,0.111652355987737,0.20499419097358,
0.299846488870027,0.394527300690664,0.396042374825994),.UNSPECIFIED.);
#610=B_SPLINE_CURVE_WITH_KNOTS('',3,(#21895,#21896,#21897,#21898,#21899,
#21900,#21901,#21902,#21903,#21904,#21905,#21906),.UNSPECIFIED.,.F.,.F.,
(4,2,2,2,2,4),(0.396042374825994,0.490876853267616,0.585866484025814,0.675498135386537,
0.761377359963428,0.770847053721237),.UNSPECIFIED.);
#611=B_SPLINE_CURVE_WITH_KNOTS('',3,(#21907,#21908,#21909,#21910,#21911,
#21912,#21913,#21914,#21915,#21916,#21917,#21918),.UNSPECIFIED.,.F.,.F.,
(4,2,2,2,2,4),(-0.727854718895878,-0.649817772706759,-0.557871466640106,
-0.462969650386807,-0.367340921859025,-0.353056606424783),.UNSPECIFIED.);
#612=B_SPLINE_CURVE_WITH_KNOTS('',3,(#21920,#21921,#21922,#21923,#21924,
#21925,#21926,#21927,#21928,#21929,#21930,#21931,#21932,#21933,#21934,#21935,
#21936,#21937,#21938,#21939,#21940,#21941,#21942,#21943,#21944,#21945,#21946,
#21947,#21948,#21949,#21950,#21951,#21952,#21953,#21954,#21955,#21956,#21957,
#21958),.UNSPECIFIED.,.T.,.F.,(4,2,2,2,2,2,2,2,2,3,2,2,2,2,2,2,2,2,4),(-0.7577515844171,
-0.736832386346907,-0.640706303106354,-0.54687575262776,-0.458462079703312,
-0.372641160637091,-0.283889834493717,-0.19079436895225,-0.096117228806511,
0.,0.0612173298619945,0.121966896291198,0.214605744640411,0.30206903695819,
0.387916805853724,0.477547309412777,0.571760843278307,0.667059100969111,
0.740952092944516),.UNSPECIFIED.);
#613=B_SPLINE_CURVE_WITH_KNOTS('',3,(#21976,#21977,#21978,#21979,#21980,
#21981,#21982,#21983,#21984,#21985),.UNSPECIFIED.,.F.,.F.,(4,2,2,2,4),(0.302390904078212,
0.377985652694416,0.453580401310619,0.529181104733521,0.604781808156423),
 .UNSPECIFIED.);
#614=B_SPLINE_CURVE_WITH_KNOTS('',3,(#21987,#21988,#21989,#21990,#21991,
#21992,#21993,#21994,#21995,#21996),.UNSPECIFIED.,.F.,.F.,(4,2,2,2,4),(0.604781808156423,
0.680382511579325,0.755983215002227,0.831577963618431,0.907172712234635),
 .UNSPECIFIED.);
#615=B_SPLINE_CURVE_WITH_KNOTS('',3,(#22000,#22001,#22002,#22003,#22004,
#22005,#22006,#22007,#22008,#22009),.UNSPECIFIED.,.F.,.F.,(4,2,2,2,4),(0.47110500506321,
0.588852659623554,0.706600314183898,0.824405162155159,0.942210010126421),
 .UNSPECIFIED.);
#616=B_SPLINE_CURVE_WITH_KNOTS('',3,(#22011,#22012,#22013,#22014,#22015,
#22016,#22017,#22018,#22019,#22020),.UNSPECIFIED.,.F.,.F.,(4,2,2,2,4),(0.942210010126421,
1.06001485809768,1.17781970606894,1.29556736062929,1.41331501518963),
 .UNSPECIFIED.);
#617=B_SPLINE_CURVE_WITH_KNOTS('',3,(#22025,#22026,#22027,#22028,#22029,
#22030,#22031,#22032,#22033,#22034),.UNSPECIFIED.,.F.,.F.,(4,2,2,2,4),(1.41331501518963,
1.53106266974997,1.64881032431032,1.76661517228158,1.88442002025284),
 .UNSPECIFIED.);
#618=B_SPLINE_CURVE_WITH_KNOTS('',3,(#22035,#22036,#22037,#22038,#22039,
#22040,#22041,#22042,#22043,#22044),.UNSPECIFIED.,.F.,.F.,(4,2,2,2,4),(0.,
0.117804847971262,0.235609695942523,0.353357350502867,0.47110500506321),
 .UNSPECIFIED.);
#619=B_SPLINE_CURVE_WITH_KNOTS('',3,(#22046,#22047,#22048,#22049,#22050,
#22051,#22052,#22053,#22054,#22055),.UNSPECIFIED.,.F.,.F.,(4,2,2,2,4),(0.907172712234635,
0.982767460850839,1.05836220946704,1.13396291288994,1.20956361631285),
 .UNSPECIFIED.);
#620=B_SPLINE_CURVE_WITH_KNOTS('',3,(#22056,#22057,#22058,#22059,#22060,
#22061,#22062,#22063,#22064,#22065),.UNSPECIFIED.,.F.,.F.,(4,2,2,2,4),(0.,
0.0756007034229019,0.151201406845804,0.226796155462008,0.302390904078212),
 .UNSPECIFIED.);
#621=B_SPLINE_CURVE_WITH_KNOTS('',3,(#22069,#22070,#22071,#22072,#22073,
#22074,#22075,#22076,#22077,#22078,#22079,#22080,#22081,#22082,#22083,#22084,
#22085,#22086,#22087,#22088,#22089,#22090,#22091,#22092,#22093,#22094,#22095),
 .UNSPECIFIED.,.F.,.F.,(4,2,2,2,3,2,2,2,2,2,2,2,4),(0.907172712234635,0.982767460850839,
1.05836220946704,1.13396291288994,1.20956361631285,1.28516431973575,1.36076502315865,
1.43635977177485,1.51195452039106,1.58754926900726,1.66314401762347,1.73874472104637,
1.81434542446927),.UNSPECIFIED.);
#622=B_SPLINE_CURVE_WITH_KNOTS('',3,(#22096,#22097,#22098,#22099,#22100,
#22101,#22102,#22103,#22104,#22105),.UNSPECIFIED.,.F.,.F.,(4,2,2,2,4),(1.81434542446927,
1.88994612789217,1.96554683131507,2.04114157993128,2.11673632854748),
 .UNSPECIFIED.);
#623=B_SPLINE_CURVE_WITH_KNOTS('',3,(#22108,#22109,#22110,#22111,#22112,
#22113,#22114,#22115,#22116,#22117,#22118,#22119,#22120,#22121,#22122,#22123,
#22124,#22125,#22126,#22127,#22128,#22129,#22130,#22131,#22132,#22133,#22134),
 .UNSPECIFIED.,.F.,.F.,(4,2,2,2,3,2,2,2,2,2,2,2,4),(1.41331501518963,1.53106266974997,
1.64881032431032,1.76661517228158,1.88442002025284,2.0022248682241,2.12002971619536,
2.23777737075571,2.35552502531605,2.4732726798764,2.59102033443674,2.708825182408,
2.82663003037926),.UNSPECIFIED.);
#624=B_SPLINE_CURVE_WITH_KNOTS('',3,(#22135,#22136,#22137,#22138,#22139,
#22140,#22141,#22142,#22143,#22144),.UNSPECIFIED.,.F.,.F.,(4,2,2,2,4),(2.82663003037926,
2.94443487835052,3.06223972632179,3.17998738088213,3.29773503544247),
 .UNSPECIFIED.);
#625=B_SPLINE_CURVE_WITH_KNOTS('',3,(#22152,#22153,#22154,#22155,#22156,
#22157,#22158,#22159,#22160,#22161,#22162,#22163,#22164,#22165,#22166,#22167,
#22168,#22169,#22170,#22171,#22172,#22173,#22174,#22175,#22176,#22177,#22178,
#22179,#22180,#22181,#22182,#22183,#22184,#22185,#22186,#22187,#22188),
 .UNSPECIFIED.,.F.,.F.,(4,2,2,2,2,2,2,2,2,2,3,2,2,2,2,2,2,4),(0.66709016003974,
0.694276778086138,0.770594476757215,0.84906692863503,0.927850026287074,
0.965860761886542,1.00385889129356,1.07985135515414,1.15830200911339,1.21149927946789,
1.26460940023701,1.3023609951576,1.34039955079445,1.37852748721988,1.41681863761144,
1.49590023217333,1.57485124143574,1.61563645580579),.UNSPECIFIED.);
#626=B_SPLINE_CURVE_WITH_KNOTS('',3,(#22190,#22191,#22192,#22193,#22194,
#22195,#22196,#22197,#22198,#22199,#22200,#22201,#22202,#22203,#22204,#22205),
 .UNSPECIFIED.,.F.,.F.,(4,2,2,2,2,2,2,4),(1.61563645580579,1.65065033370949,
1.72635516248862,1.80489182430705,1.84434548324305,1.88293297920974,1.92132794397062,
1.93169956027675),.UNSPECIFIED.);
#627=B_SPLINE_CURVE_WITH_KNOTS('',3,(#22210,#22211,#22212,#22213,#22214,
#22215,#22216,#22217,#22218,#22219,#22220,#22221,#22222,#22223,#22224,#22225,
#22226,#22227,#22228,#22229),.UNSPECIFIED.,.F.,.F.,(4,2,2,2,2,2,2,2,2,4),
(1.26878286228387,1.3415697328015,1.4185184514642,1.49730235790989,1.57510611204151,
1.6512168301348,1.7286733175368,1.80824177624455,1.84722443352035,1.90183587401007),
 .UNSPECIFIED.);
#628=B_SPLINE_CURVE_WITH_KNOTS('',3,(#22230,#22231,#22232,#22233,#22234,
#22235,#22236,#22237,#22238,#22239,#22240,#22241,#22242,#22243,#22244,#22245,
#22246,#22247,#22248,#22249,#22250,#22251,#22252,#22253,#22254,#22255,#22256,
#22257,#22258,#22259,#22260),.UNSPECIFIED.,.F.,.F.,(4,2,2,2,2,2,2,2,2,2,
2,2,2,3,4),(0.636510547675982,0.658871161538065,0.696960874037515,0.735081814971663,
0.813573460248337,0.833402362698247,0.872507027375637,0.911354700684223,
0.98788468247215,1.02607483553733,1.06428112645553,1.14327310095656,1.20431912927923,
1.26532532633409,1.26878286228387),.UNSPECIFIED.);
#629=B_SPLINE_CURVE_WITH_KNOTS('',1,(#23311,#23312),.UNSPECIFIED.,.F.,.F.,
(2,2),(-0.999999999999999,-7.62951798228629E-16),.UNSPECIFIED.);
#630=B_SPLINE_CURVE_WITH_KNOTS('',1,(#23765,#23766),.UNSPECIFIED.,.F.,.F.,
(2,2),(-1.,3.41544860156615E-16),.UNSPECIFIED.);
#631=B_SPLINE_CURVE_WITH_KNOTS('',3,(#23782,#23783,#23784,#23785,#23786,
#23787,#23788,#23789,#23790,#23791),.UNSPECIFIED.,.F.,.F.,(4,2,2,2,4),(-0.321465265823507,
-0.241103193298965,-0.160741120774423,-0.0803705603872117,0.),
 .UNSPECIFIED.);
#632=B_SPLINE_CURVE_WITH_KNOTS('',3,(#23793,#23794,#23795,#23796,#23797,
#23798,#23799,#23800,#23801,#23802),.UNSPECIFIED.,.F.,.F.,(4,2,2,2,4),(0.,
0.0803705603872116,0.160741120774423,0.241103193298965,0.321465265823507),
 .UNSPECIFIED.);
#633=B_SPLINE_CURVE_WITH_KNOTS('',3,(#23807,#23808,#23809,#23810,#23811,
#23812,#23813,#23814,#23815,#23816),.UNSPECIFIED.,.F.,.F.,(4,2,2,2,4),(0.321465265823507,
0.401827338348048,0.48218941087259,0.562559971259802,0.642930531647013),
 .UNSPECIFIED.);
#634=B_SPLINE_CURVE_WITH_KNOTS('',3,(#23817,#23818,#23819,#23820,#23821,
#23822,#23823,#23824,#23825,#23826),.UNSPECIFIED.,.F.,.F.,(4,2,2,2,4),(-0.642930531647014,
-0.562559971259802,-0.48218941087259,-0.401827338348049,-0.321465265823507),
 .UNSPECIFIED.);
#635=B_SPLINE_CURVE_WITH_KNOTS('',3,(#23829,#23830,#23831,#23832,#23833,
#23834,#23835,#23836,#23837,#23838),.UNSPECIFIED.,.F.,.F.,(4,2,2,2,4),(0.96439579747052,
1.04475786999506,1.1251199425196,1.20549050290682,1.28586106329403),
 .UNSPECIFIED.);
#636=B_SPLINE_CURVE_WITH_KNOTS('',3,(#23839,#23840,#23841,#23842,#23843,
#23844,#23845,#23846,#23847,#23848,#23849,#23850,#23851,#23852,#23853,#23854,
#23855,#23856,#23857,#23858,#23859,#23860,#23861,#23862,#23863,#23864),
 .UNSPECIFIED.,.F.,.F.,(4,2,2,2,2,2,2,2,2,2,2,2,4),(1.28586106329403,1.36623162368124,
1.44660218406845,1.52696425659299,1.60732632911753,1.68768840164208,1.76805047416662,
1.84842103455383,1.92879159494104,2.00916215532825,2.08953271571546,2.16989478824001,
2.25025686076455),.UNSPECIFIED.);
#637=B_SPLINE_CURVE_WITH_KNOTS('',3,(#27616,#27617,#27618,#27619,#27620,
#27621,#27622,#27623,#27624,#27625,#27626,#27627,#27628,#27629,#27630,#27631,
#27632,#27633,#27634,#27635,#27636,#27637,#27638,#27639,#27640,#27641,#27642,
#27643,#27644,#27645,#27646,#27647,#27648,#27649,#27650,#27651,#27652,#27653,
#27654,#27655,#27656,#27657,#27658,#27659,#27660,#27661,#27662,#27663,#27664,
#27665,#27666,#27667,#27668,#27669),.UNSPECIFIED.,.F.,.F.,(4,2,2,2,2,2,
2,2,2,2,2,2,2,2,2,2,2,2,2,2,2,2,2,2,2,2,4),(0.,0.211530220655383,0.289081942912891,
0.502162303944745,0.617685523778197,0.735044758583038,1.02805780346695,
1.42592405474646,1.85809441022839,1.99080242607033,2.05848328284043,2.1001327114057,
2.13819962143761,2.18412793694465,2.26153227088293,2.41592184272421,2.86718043954418,
3.43208938067713,4.01802145807674,4.65968133801718,5.38245910771257,5.56242601552907,
6.27810834200945,6.60236241786042,7.05771390645932,7.27425164190709,7.48648678308462),
 .UNSPECIFIED.);
#638=B_SPLINE_CURVE_WITH_KNOTS('',3,(#27670,#27671,#27672,#27673,#27674,
#27675,#27676,#27677,#27678,#27679,#27680,#27681,#27682,#27683,#27684,#27685,
#27686,#27687,#27688,#27689,#27690,#27691,#27692,#27693,#27694,#27695,#27696,
#27697,#27698,#27699,#27700,#27701,#27702,#27703,#27704,#27705,#27706,#27707,
#27708,#27709,#27710,#27711,#27712,#27713,#27714,#27715,#27716,#27717,#27718,
#27719,#27720,#27721,#27722,#27723,#27724,#27725),.UNSPECIFIED.,.F.,.F.,
(4,2,2,2,2,2,2,2,2,2,2,2,2,2,2,2,2,2,2,2,2,2,2,2,2,2,2,4),(0.,0.0508933598535436,
0.102714861816748,0.211107408796559,0.288664279862181,0.501758787708079,
0.617289677349956,0.734656703859758,1.02768920244262,1.42558186882727,1.85778091692665,
1.99049774351539,2.05818309375797,2.09983528751381,2.1379047248868,2.18383608967027,
2.26124556263954,2.41564538471522,2.86693394150261,3.43188038808134,4.01785136669594,
4.65955384773215,5.38237960410595,5.56235846028945,6.27808830236667,6.60236390610103,
7.05774562640548,7.48689591445956),.UNSPECIFIED.);
#639=B_SPLINE_CURVE_WITH_KNOTS('',3,(#28035,#28036,#28037,#28038,#28039,
#28040,#28041,#28042),.UNSPECIFIED.,.F.,.F.,(4,2,2,4),(-0.269775582616464,
-0.253421285918584,-0.22590943032474,-0.222790814239488),.UNSPECIFIED.);
#640=B_SPLINE_CURVE_WITH_KNOTS('',3,(#28046,#28047,#28048,#28049,#28050,
#28051),.UNSPECIFIED.,.F.,.F.,(4,2,4),(-0.0146617576038819,-0.00732399879407159,
0.),.UNSPECIFIED.);
#641=B_SPLINE_CURVE_WITH_KNOTS('',3,(#28055,#28056,#28057,#28058,#28059,
#28060),.UNSPECIFIED.,.F.,.F.,(4,2,4),(-0.0146584345608506,-0.00733705776971509,
-2.0365131182774E-6),.UNSPECIFIED.);
#642=B_SPLINE_CURVE_WITH_KNOTS('',3,(#28063,#28064,#28065,#28066,#28067,
#28068),.UNSPECIFIED.,.F.,.F.,(4,2,4),(-0.131101349644823,-0.108436635501131,
-0.0855680085348876),.UNSPECIFIED.);
#643=B_SPLINE_CURVE_WITH_KNOTS('',3,(#28074,#28075,#28076,#28077,#28078,
#28079),.UNSPECIFIED.,.F.,.F.,(4,2,4),(-0.131101349644766,-0.108436635501081,
-0.0855680085348502),.UNSPECIFIED.);
#644=B_SPLINE_CURVE_WITH_KNOTS('',3,(#28083,#28084,#28085,#28086,#28087,
#28088,#28089,#28090),.UNSPECIFIED.,.F.,.F.,(4,2,2,4),(-0.269775582616478,
-0.253421285918598,-0.225909430324752,-0.222790814239499),.UNSPECIFIED.);
#645=B_SPLINE_CURVE_WITH_KNOTS('',3,(#28094,#28095,#28096,#28097,#28098,
#28099),.UNSPECIFIED.,.F.,.F.,(4,2,4),(-0.0146618387590922,-0.00732404409132206,
-1.5273897580742E-8),.UNSPECIFIED.);
#646=B_SPLINE_CURVE_WITH_KNOTS('',3,(#28102,#28103,#28104,#28105,#28106,
#28107),.UNSPECIFIED.,.F.,.F.,(4,2,4),(-0.0146570227865704,-0.00733642775269209,
-9.89091544272014E-7),.UNSPECIFIED.);
#647=B_SPLINE_CURVE_WITH_KNOTS('',3,(#28113,#28114,#28115,#28116,#28117,
#28118),.UNSPECIFIED.,.F.,.F.,(4,2,4),(-0.131101349644767,-0.108436635501072,
-0.0855680085348483),.UNSPECIFIED.);
#648=B_SPLINE_CURVE_WITH_KNOTS('',3,(#28122,#28123,#28124,#28125,#28126,
#28127,#28128,#28129),.UNSPECIFIED.,.F.,.F.,(4,2,2,4),(-0.269775582616373,
-0.253421285918502,-0.225909430324671,-0.222790814239419),.UNSPECIFIED.);
#649=B_SPLINE_CURVE_WITH_KNOTS('',3,(#28133,#28134,#28135,#28136,#28137,
#28138),.UNSPECIFIED.,.F.,.F.,(4,2,4),(-0.0146618152090308,-0.00732403346802824,
-1.542284065216E-8),.UNSPECIFIED.);
#650=B_SPLINE_CURVE_WITH_KNOTS('',3,(#28141,#28142,#28143,#28144,#28145,
#28146),.UNSPECIFIED.,.F.,.F.,(4,2,4),(-0.0146570266562873,-0.00733642653042715,
-9.88349770934815E-7),.UNSPECIFIED.);
#651=B_SPLINE_CURVE_WITH_KNOTS('',3,(#28152,#28153,#28154,#28155,#28156,
#28157),.UNSPECIFIED.,.F.,.F.,(4,2,4),(-0.131101349644736,-0.108436635501052,
-0.0855680085348304),.UNSPECIFIED.);
#652=B_SPLINE_CURVE_WITH_KNOTS('',3,(#28161,#28162,#28163,#28164,#28165,
#28166,#28167,#28168),.UNSPECIFIED.,.F.,.F.,(4,2,2,4),(-0.269775582616424,
-0.25342128591855,-0.225909430324718,-0.222790814239467),.UNSPECIFIED.);
#653=B_SPLINE_CURVE_WITH_KNOTS('',3,(#28172,#28173,#28174,#28175,#28176,
#28177),.UNSPECIFIED.,.F.,.F.,(4,2,4),(-0.01466175760385,-0.00732399879408571,
0.),.UNSPECIFIED.);
#654=B_SPLINE_CURVE_WITH_KNOTS('',3,(#28182,#28183,#28184,#28185,#28186,
#28187),.UNSPECIFIED.,.F.,.F.,(4,2,4),(-0.0146584345606624,-0.00733705776964583,
-2.03651308581504E-6),.UNSPECIFIED.);
#655=B_SPLINE_CURVE_WITH_KNOTS('',3,(#28193,#28194,#28195,#28196,#28197,
#28198,#28199,#28200),.UNSPECIFIED.,.F.,.F.,(4,2,2,4),(-0.269775582616442,
-0.253421285918564,-0.225909430324722,-0.22279081423947),.UNSPECIFIED.);
#656=B_SPLINE_CURVE_WITH_KNOTS('',3,(#28204,#28205,#28206,#28207,#28208,
#28209),.UNSPECIFIED.,.F.,.F.,(4,2,4),(-0.0146618387596521,-0.0073240440914945,
-1.52738934607738E-8),.UNSPECIFIED.);
#657=B_SPLINE_CURVE_WITH_KNOTS('',3,(#28213,#28214,#28215,#28216,#28217,
#28218),.UNSPECIFIED.,.F.,.F.,(4,2,4),(-0.0146570266563023,-0.00733642653042518,
-9.88349766483515E-7),.UNSPECIFIED.);
#658=B_SPLINE_CURVE_WITH_KNOTS('',3,(#28221,#28222,#28223,#28224,#28225,
#28226),.UNSPECIFIED.,.F.,.F.,(4,2,4),(-0.131101349644881,-0.108436635501189,
-0.0855680085349263),.UNSPECIFIED.);
#659=B_SPLINE_CURVE_WITH_KNOTS('',3,(#28232,#28233,#28234,#28235,#28236,
#28237),.UNSPECIFIED.,.F.,.F.,(4,2,4),(-0.131101349644726,-0.108436635501036,
-0.0855680085348208),.UNSPECIFIED.);
#660=B_SPLINE_CURVE_WITH_KNOTS('',3,(#28241,#28242,#28243,#28244,#28245,
#28246,#28247,#28248),.UNSPECIFIED.,.F.,.F.,(4,2,2,4),(-0.26977558261646,
-0.253421285918579,-0.225909430324732,-0.222790814239478),.UNSPECIFIED.);
#661=B_SPLINE_CURVE_WITH_KNOTS('',3,(#28252,#28253,#28254,#28255,#28256,
#28257),.UNSPECIFIED.,.F.,.F.,(4,2,4),(-0.01466175760387,-0.0073239987940538,
0.),.UNSPECIFIED.);
#662=B_SPLINE_CURVE_WITH_KNOTS('',3,(#28260,#28261,#28262,#28263,#28264,
#28265),.UNSPECIFIED.,.F.,.F.,(4,2,4),(-0.0146584345608046,-0.00733705776969051,
-2.03651309724679E-6),.UNSPECIFIED.);
#663=B_SPLINE_CURVE_WITH_KNOTS('',3,(#28271,#28272,#28273,#28274,#28275,
#28276),.UNSPECIFIED.,.F.,.F.,(4,2,4),(-0.131101349644819,-0.108436635501123,
-0.0855680085348801),.UNSPECIFIED.);
#664=B_SPLINE_CURVE_WITH_KNOTS('',3,(#28280,#28281,#28282,#28283,#28284,
#28285,#28286,#28287),.UNSPECIFIED.,.F.,.F.,(4,2,2,4),(-0.269775582616506,
-0.253421285918626,-0.225909430324778,-0.222790814239526),.UNSPECIFIED.);
#665=B_SPLINE_CURVE_WITH_KNOTS('',3,(#28291,#28292,#28293,#28294,#28295,
#28296),.UNSPECIFIED.,.F.,.F.,(4,2,4),(-0.0146618387590248,-0.00732404409122351,
-1.52738976744171E-8),.UNSPECIFIED.);
#666=B_SPLINE_CURVE_WITH_KNOTS('',3,(#28299,#28300,#28301,#28302,#28303,
#28304),.UNSPECIFIED.,.F.,.F.,(4,2,4),(-0.0146570227863867,-0.00733642775264506,
-9.89091543862619E-7),.UNSPECIFIED.);
#667=B_SPLINE_CURVE_WITH_KNOTS('',3,(#28310,#28311,#28312,#28313,#28314,
#28315),.UNSPECIFIED.,.F.,.F.,(4,2,4),(-0.131101349644802,-0.108436635501105,
-0.0855680085348711),.UNSPECIFIED.);
#668=B_SPLINE_CURVE_WITH_KNOTS('',3,(#28319,#28320,#28321,#28322,#28323,
#28324,#28325,#28326),.UNSPECIFIED.,.F.,.F.,(4,2,2,4),(-0.269775582616408,
-0.253421285918538,-0.225909430324714,-0.222790814239463),.UNSPECIFIED.);
#669=B_SPLINE_CURVE_WITH_KNOTS('',3,(#28330,#28331,#28332,#28333,#28334,
#28335),.UNSPECIFIED.,.F.,.F.,(4,2,4),(-0.0146618152087878,-0.00732403346791597,
-1.54228420676944E-8),.UNSPECIFIED.);
#670=B_SPLINE_CURVE_WITH_KNOTS('',3,(#28338,#28339,#28340,#28341,#28342,
#28343),.UNSPECIFIED.,.F.,.F.,(4,2,4),(-0.0146570266560919,-0.00733642653037241,
-9.88349764358479E-7),.UNSPECIFIED.);
#671=B_SPLINE_CURVE_WITH_KNOTS('',3,(#28349,#28350,#28351,#28352,#28353,
#28354),.UNSPECIFIED.,.F.,.F.,(4,2,4),(-0.131101349644797,-0.108436635501117,
-0.0855680085348727),.UNSPECIFIED.);
#672=B_SPLINE_CURVE_WITH_KNOTS('',3,(#28358,#28359,#28360,#28361,#28362,
#28363,#28364,#28365),.UNSPECIFIED.,.F.,.F.,(4,2,2,4),(-0.269775582616456,
-0.253421285918579,-0.225909430324743,-0.222790814239492),.UNSPECIFIED.);
#673=B_SPLINE_CURVE_WITH_KNOTS('',3,(#28369,#28370,#28371,#28372,#28373,
#28374),.UNSPECIFIED.,.F.,.F.,(4,2,4),(-0.0146617576042861,-0.00732399879426565,
0.),.UNSPECIFIED.);
#674=B_SPLINE_CURVE_WITH_KNOTS('',3,(#28377,#28378,#28379,#28380,#28381,
#28382),.UNSPECIFIED.,.F.,.F.,(4,2,4),(-0.0146584345607558,-0.00733705776967299,
-2.03651308879836E-6),.UNSPECIFIED.);
#675=B_SPLINE_CURVE_WITH_KNOTS('',3,(#28415,#28416,#28417,#28418,#28419,
#28420),.UNSPECIFIED.,.F.,.F.,(4,2,4),(-0.131101349644817,-0.108436635501125,
-0.085568008534881),.UNSPECIFIED.);
#676=B_SPLINE_CURVE_WITH_KNOTS('',3,(#28422,#28423,#28424,#28425,#28426,
#28427,#28428,#28429),.UNSPECIFIED.,.F.,.F.,(4,2,2,4),(-0.269775582616367,
-0.253421285918495,-0.225909430324662,-0.222790814239412),.UNSPECIFIED.);
#677=B_SPLINE_CURVE_WITH_KNOTS('',3,(#28433,#28434,#28435,#28436,#28437,
#28438),.UNSPECIFIED.,.F.,.F.,(4,2,4),(-0.0146618387595114,-0.00732404409148471,
-1.52738936567975E-8),.UNSPECIFIED.);
#678=B_SPLINE_CURVE_WITH_KNOTS('',3,(#28441,#28442,#28443,#28444,#28445,
#28446),.UNSPECIFIED.,.F.,.F.,(4,2,4),(-0.0146570266563214,-0.00733642653043949,
-9.88349770927877E-7),.UNSPECIFIED.);
#679=B_SPLINE_CURVE_WITH_KNOTS('',3,(#28464,#28465,#28466,#28467,#28468,
#28469,#28470,#28471,#28472,#28473,#28474,#28475,#28476,#28477,#28478,#28479,
#28480,#28481),.UNSPECIFIED.,.F.,.F.,(4,2,2,2,2,2,2,2,4),(-1.13175700460039,
-1.06102166552592,-0.99028632645144,-0.919552039950867,-0.848817753450294,
-0.77808346694972,-0.707349180449147,-0.636613841374672,-0.565878502300197),
 .UNSPECIFIED.);
#680=B_SPLINE_CURVE_WITH_KNOTS('',3,(#28482,#28483,#28484,#28485,#28486,
#28487,#28488,#28489,#28490,#28491,#28492,#28493,#28494,#28495,#28496,#28497,
#28498,#28499),.UNSPECIFIED.,.F.,.F.,(4,2,2,2,2,2,2,2,4),(-0.565878502300197,
-0.495143163225721,-0.424407824151245,-0.353673537650672,-0.282939251150098,
-0.212204964649525,-0.141470678148952,-0.0707353390744758,0.),
 .UNSPECIFIED.);
#681=B_SPLINE_CURVE_WITH_KNOTS('',3,(#28502,#28503,#28504,#28505,#28506,
#28507,#28508,#28509,#28510,#28511,#28512,#28513,#28514,#28515,#28516,#28517,
#28518,#28519),.UNSPECIFIED.,.F.,.F.,(4,2,2,2,2,2,2,2,4),(-1.13175700460039,
-1.06102166552592,-0.990286326451441,-0.919552039950867,-0.848817753450294,
-0.778083466949721,-0.707349180449147,-0.636613841374672,-0.565878502300197),
 .UNSPECIFIED.);
#682=B_SPLINE_CURVE_WITH_KNOTS('',3,(#28520,#28521,#28522,#28523,#28524,
#28525,#28526,#28527,#28528,#28529,#28530,#28531,#28532,#28533,#28534,#28535,
#28536,#28537),.UNSPECIFIED.,.F.,.F.,(4,2,2,2,2,2,2,2,4),(-0.565878502300197,
-0.495143163225721,-0.424407824151246,-0.353673537650672,-0.282939251150099,
-0.212204964649525,-0.141470678148952,-0.070735339074476,0.),
 .UNSPECIFIED.);
#683=B_SPLINE_CURVE_WITH_KNOTS('',3,(#28540,#28541,#28542,#28543,#28544,
#28545,#28546,#28547,#28548,#28549,#28550,#28551,#28552,#28553,#28554,#28555,
#28556,#28557),.UNSPECIFIED.,.F.,.F.,(4,2,2,2,2,2,2,2,4),(-1.13175700460039,
-1.06102166552592,-0.990286326451441,-0.919552039950867,-0.848817753450294,
-0.77808346694972,-0.707349180449147,-0.636613841374672,-0.565878502300197),
 .UNSPECIFIED.);
#684=B_SPLINE_CURVE_WITH_KNOTS('',3,(#28558,#28559,#28560,#28561,#28562,
#28563,#28564,#28565,#28566,#28567,#28568,#28569,#28570,#28571,#28572,#28573,
#28574,#28575),.UNSPECIFIED.,.F.,.F.,(4,2,2,2,2,2,2,2,4),(-0.565878502300197,
-0.495143163225721,-0.424407824151245,-0.353673537650672,-0.282939251150098,
-0.212204964649525,-0.141470678148952,-0.0707353390744758,0.),
 .UNSPECIFIED.);
#685=B_SPLINE_CURVE_WITH_KNOTS('',3,(#28578,#28579,#28580,#28581,#28582,
#28583,#28584,#28585,#28586,#28587,#28588,#28589,#28590,#28591,#28592,#28593,
#28594,#28595),.UNSPECIFIED.,.F.,.F.,(4,2,2,2,2,2,2,2,4),(-1.1317570046004,
-1.06102166552592,-0.990286326451445,-0.919552039950871,-0.848817753450298,
-0.778083466949725,-0.707349180449151,-0.636613841374674,-0.565878502300198),
 .UNSPECIFIED.);
#686=B_SPLINE_CURVE_WITH_KNOTS('',3,(#28596,#28597,#28598,#28599,#28600,
#28601,#28602,#28603,#28604,#28605,#28606,#28607,#28608,#28609,#28610,#28611,
#28612,#28613),.UNSPECIFIED.,.F.,.F.,(4,2,2,2,2,2,2,2,4),(-0.565878502300198,
-0.495143163225722,-0.424407824151246,-0.353673537650672,-0.282939251150099,
-0.212204964649525,-0.141470678148952,-0.0707353390744759,0.),
 .UNSPECIFIED.);
#687=B_SPLINE_CURVE_WITH_KNOTS('',3,(#28616,#28617,#28618,#28619,#28620,
#28621,#28622,#28623,#28624,#28625,#28626,#28627,#28628,#28629,#28630,#28631,
#28632,#28633),.UNSPECIFIED.,.F.,.F.,(4,2,2,2,2,2,2,2,4),(-0.848817753450289,
-0.778083466949716,-0.707349180449143,-0.636613841374668,-0.565878502300194,
-0.495143163225718,-0.424407824151242,-0.353673537650669,-0.282939251150097),
 .UNSPECIFIED.);
#688=B_SPLINE_CURVE_WITH_KNOTS('',3,(#28634,#28635,#28636,#28637,#28638,
#28639,#28640,#28641,#28642,#28643,#28644,#28645,#28646,#28647,#28648,#28649,
#28650,#28651,#28652),.UNSPECIFIED.,.F.,.F.,(4,2,2,2,3,2,2,2,4),(-0.282939251150097,
-0.212204964649524,-0.141470678148952,-0.0707353390744758,0.,0.0707353390744749,
0.14147067814895,0.212204964649523,0.282939251150096),.UNSPECIFIED.);
#689=B_SPLINE_CURVE_WITH_KNOTS('',3,(#28663,#28664,#28665,#28666,#28667,
#28668,#28669,#28670,#28671,#28672,#28673,#28674,#28675,#28676,#28677,#28678,
#28679,#28680,#28681,#28682,#28683,#28684),.UNSPECIFIED.,.F.,.F.,(4,2,2,
2,2,2,2,2,2,2,4),(1.03259187272008E-9,0.000910225950447462,0.00182045190089492,
0.00227556487611866,0.00273067785134239,0.00364090380178987,0.00409601677701361,
0.00455112975223734,0.00546135570268482,0.0063715816531323,0.00728180748389903),
 .UNSPECIFIED.);
#690=B_SPLINE_CURVE_WITH_KNOTS('',3,(#28685,#28686,#28687,#28688,#28689,
#28690,#28691,#28692,#28693,#28694,#28695,#28696,#28697,#28698,#28699,#28700,
#28701,#28702,#28703,#28704,#28705,#28706,#28707,#28708,#28709,#28710,#28711,
#28712,#28713,#28714,#28715,#28716,#28717,#28718,#28719,#28720,#28721,#28722,
#28723,#28724,#28725,#28726,#28727,#28728,#28729,#28730,#28731,#28732,#28733,
#28734,#28735,#28736,#28737,#28738,#28739,#28740,#28741,#28742,#28743,#28744,
#28745,#28746,#28747,#28748,#28749,#28750,#28751,#28752,#28753,#28754,#28755,
#28756,#28757,#28758,#28759,#28760,#28761,#28762,#28763,#28764,#28765,#28766,
#28767,#28768,#28769),.UNSPECIFIED.,.F.,.F.,(4,3,3,3,3,3,3,3,3,3,3,3,3,
3,3,3,3,3,3,3,3,3,3,3,3,3,3,3,4),(1.27326789064134E-9,0.000305183030961356,
0.000618697405666451,0.000865973237167131,0.000907586176443212,0.00143258173570116,
0.00178321767141052,0.00181517235288642,0.00233679237650043,0.00270521777421962,
0.00272275852932964,0.0031677449805063,0.00317655161755125,0.00351188758019002,
0.00363034470577285,0.00363091529585842,0.00404743389245343,0.00446889752821537,
0.00453793088221607,0.00455651100281011,0.00512035053921118,0.00544551705865929,
0.00547872254023125,0.00584209036189708,0.00622546925989105,0.00635310323510251,
0.00664528416315127,0.00695298625517416,0.00726068834719705),
 .UNSPECIFIED.);
#691=B_SPLINE_CURVE_WITH_KNOTS('',3,(#28770,#28771,#28772,#28773,#28774,
#28775,#28776,#28777,#28778,#28779,#28780,#28781,#28782,#28783,#28784,#28785,
#28786,#28787,#28788,#28789,#28790,#28791),.UNSPECIFIED.,.F.,.F.,(4,2,2,
2,2,2,2,2,2,2,4),(1.03259179694757E-9,0.000910225950447464,0.00182045190089493,
0.00227556487611866,0.0027306778513424,0.00364090380178987,0.00409601677701361,
0.00455112975223735,0.00546135570268482,0.00637158165313229,0.00728180748389901),
 .UNSPECIFIED.);
#692=B_SPLINE_CURVE_WITH_KNOTS('',3,(#28792,#28793,#28794,#28795,#28796,
#28797,#28798,#28799,#28800,#28801,#28802,#28803,#28804,#28805,#28806,#28807,
#28808,#28809,#28810,#28811,#28812,#28813,#28814,#28815,#28816,#28817,#28818,
#28819,#28820,#28821,#28822,#28823,#28824,#28825,#28826,#28827,#28828,#28829,
#28830,#28831,#28832,#28833,#28834,#28835,#28836,#28837,#28838,#28839,#28840,
#28841,#28842,#28843,#28844,#28845,#28846,#28847,#28848,#28849,#28850,#28851,
#28852,#28853,#28854,#28855,#28856,#28857,#28858,#28859,#28860,#28861,#28862,
#28863,#28864,#28865,#28866,#28867,#28868,#28869,#28870,#28871,#28872,#28873),
 .UNSPECIFIED.,.F.,.F.,(4,3,3,3,3,3,3,3,3,3,3,3,3,3,3,3,3,3,3,3,3,3,3,3,
3,3,3,4),(1.28482073593457E-9,0.000305235153235769,0.000618823755187696,
0.000867705358119334,0.000909427513427647,0.00143855251726445,0.00178678626263729,
0.00181885502685529,0.00234189634471885,0.00271063977086651,0.00272828254028294,
0.00317414461806316,0.00358630275067258,0.00363771005371059,0.00363819037736454,
0.00409242381042441,0.00410208104893608,0.00444871693184629,0.00454713756713824,
0.0045656013242579,0.00518563856811733,0.00545656508056589,0.00548920795128179,
0.00599393750643838,0.00636599259399354,0.0064075598747639,0.00686713671046424,
0.00727541997337556),.UNSPECIFIED.);
#693=B_SPLINE_CURVE_WITH_KNOTS('',3,(#28874,#28875,#28876,#28877,#28878,
#28879,#28880,#28881,#28882,#28883,#28884,#28885,#28886,#28887,#28888,#28889,
#28890,#28891,#28892,#28893,#28894,#28895,#28896,#28897,#28898,#28899,#28900,
#28901,#28902,#28903,#28904,#28905,#28906,#28907,#28908,#28909,#28910,#28911,
#28912,#28913,#28914,#28915,#28916,#28917,#28918,#28919,#28920,#28921,#28922,
#28923,#28924,#28925,#28926,#28927,#28928,#28929,#28930,#28931,#28932,#28933,
#28934,#28935,#28936,#28937,#28938,#28939,#28940,#28941,#28942,#28943,#28944,
#28945,#28946,#28947,#28948,#28949,#28950,#28951,#28952,#28953,#28954,#28955,
#28956,#28957,#28958),.UNSPECIFIED.,.F.,.F.,(4,3,3,3,3,3,3,3,3,3,3,3,3,
3,3,3,3,3,3,3,3,3,3,3,3,3,3,3,4),(1.27326809408661E-9,0.00030518303086706,
0.000618697405474252,0.000865973237167092,0.000907586176443212,0.0014325817372093,
0.0017832176714105,0.00181517235288642,0.00233679237665264,0.00270521777421962,
0.00272275852932964,0.0031677449805063,0.00317655161755124,0.00351188758016664,
0.00363034470577285,0.00363091529585842,0.00404743389252427,0.00446889752836537,
0.00453793088221607,0.0045565110028101,0.00512035053941143,0.00544551705865929,
0.00547872254023127,0.00584209036189159,0.00622546925988722,0.00635310323510251,
0.00664528416314683,0.00695298625517191,0.007260688347197),
 .UNSPECIFIED.);
#694=B_SPLINE_CURVE_WITH_KNOTS('',3,(#28959,#28960,#28961,#28962,#28963,
#28964,#28965,#28966,#28967,#28968,#28969,#28970,#28971,#28972,#28973,#28974,
#28975,#28976,#28977,#28978,#28979,#28980),.UNSPECIFIED.,.F.,.F.,(4,2,2,
2,2,2,2,2,2,2,4),(1.03259185302256E-9,0.000910225950447462,0.00182045190089492,
0.00227556487611866,0.00273067785134239,0.00364090380178986,0.0040960167770136,
0.00455112975223734,0.00546135570268482,0.00637158165313229,0.00728180748389903),
 .UNSPECIFIED.);
#695=B_SPLINE_CURVE_WITH_KNOTS('',3,(#28981,#28982,#28983,#28984,#28985,
#28986,#28987,#28988,#28989,#28990,#28991,#28992,#28993,#28994,#28995,#28996,
#28997,#28998,#28999,#29000,#29001,#29002,#29003,#29004,#29005,#29006,#29007,
#29008,#29009,#29010,#29011,#29012,#29013,#29014,#29015,#29016,#29017,#29018,
#29019,#29020,#29021,#29022,#29023,#29024,#29025,#29026,#29027,#29028,#29029,
#29030,#29031,#29032,#29033,#29034,#29035,#29036,#29037,#29038,#29039,#29040,
#29041,#29042,#29043,#29044,#29045,#29046,#29047,#29048,#29049,#29050,#29051,
#29052,#29053,#29054,#29055,#29056,#29057,#29058,#29059,#29060,#29061,#29062,
#29063,#29064,#29065),.UNSPECIFIED.,.F.,.F.,(4,3,3,3,3,3,3,3,3,3,3,3,3,
3,3,3,3,3,3,3,3,3,3,3,3,3,3,3,4),(1.27326788952501E-9,0.000305183030980495,
0.000618697405702965,0.000865973237167141,0.00090758617644321,0.00143258173545336,
0.00178321767141052,0.00181517235288642,0.00233679237666166,0.00270521777421961,
0.00272275852932963,0.0031677449805063,0.00317655161755124,0.00351188757989355,
0.00363034470577285,0.00363091529585842,0.00404743389254553,0.00446889752840383,
0.00453793088221607,0.0045565110028101,0.00512035054042042,0.00544551705865929,
0.00547872254023124,0.00584209036187272,0.00622546925982432,0.00635310323510251,
0.00664528416315582,0.00695298625517646,0.0072606883471971),
 .UNSPECIFIED.);
#696=B_SPLINE_CURVE_WITH_KNOTS('',3,(#29067,#29068,#29069,#29070,#29071,
#29072,#29073,#29074,#29075,#29076,#29077,#29078,#29079,#29080,#29081,#29082,
#29083,#29084,#29085,#29086,#29087,#29088),.UNSPECIFIED.,.F.,.F.,(4,2,2,
2,2,2,2,2,2,2,4),(1.03259182419686E-9,0.000910225950447465,0.00182045190089493,
0.00227556487611866,0.0027306778513424,0.00364090380178987,0.00409601677701361,
0.00455112975223735,0.00546135570268482,0.00637158165313229,0.00728180748389904),
 .UNSPECIFIED.);
#697=B_SPLINE_CURVE_WITH_KNOTS('',3,(#29089,#29090,#29091,#29092,#29093,
#29094,#29095,#29096,#29097,#29098,#29099,#29100,#29101,#29102,#29103,#29104,
#29105,#29106,#29107,#29108,#29109,#29110,#29111,#29112,#29113,#29114,#29115,
#29116,#29117,#29118,#29119,#29120,#29121,#29122,#29123,#29124,#29125,#29126,
#29127,#29128,#29129,#29130,#29131,#29132,#29133,#29134,#29135,#29136,#29137,
#29138,#29139,#29140,#29141,#29142,#29143,#29144,#29145,#29146,#29147,#29148,
#29149,#29150,#29151,#29152,#29153,#29154,#29155,#29156,#29157,#29158,#29159,
#29160,#29161,#29162,#29163,#29164,#29165,#29166,#29167,#29168,#29169,#29170),
 .UNSPECIFIED.,.F.,.F.,(4,3,3,3,3,3,3,3,3,3,3,3,3,3,3,3,3,3,3,3,3,3,3,3,
3,3,3,4),(1.28482065261636E-9,0.000305235153155936,0.000618823755024699,
0.000867705358119319,0.000909427513427649,0.00143855251661484,0.00178678626263731,
0.0018188550268553,0.00234189634486621,0.0027106397708665,0.00272828254028295,
0.00317414461806298,0.00358630275051328,0.0036377100537106,0.00363819037736455,
0.00409242381042442,0.0041020810489361,0.0044487169314161,0.00454713756713825,
0.00456560132425793,0.00518563856945916,0.00545656508056589,0.00548920795128181,
0.00599393750639588,0.00636599259399354,0.00640755987476391,0.00686713671060239,
0.00727541997337555),.UNSPECIFIED.);
#698=B_SPLINE_CURVE_WITH_KNOTS('',3,(#29171,#29172,#29173,#29174,#29175,
#29176,#29177,#29178,#29179,#29180,#29181,#29182,#29183,#29184,#29185,#29186,
#29187,#29188,#29189,#29190,#29191,#29192,#29193,#29194,#29195,#29196,#29197,
#29198,#29199,#29200,#29201,#29202,#29203,#29204,#29205,#29206,#29207,#29208,
#29209,#29210,#29211,#29212,#29213,#29214,#29215,#29216,#29217,#29218,#29219,
#29220,#29221,#29222,#29223,#29224,#29225,#29226,#29227,#29228,#29229,#29230,
#29231,#29232,#29233,#29234,#29235,#29236,#29237,#29238,#29239,#29240,#29241,
#29242,#29243,#29244,#29245,#29246,#29247,#29248,#29249,#29250,#29251,#29252,
#29253,#29254,#29255),.UNSPECIFIED.,.F.,.F.,(4,3,3,3,3,3,3,3,3,3,3,3,3,
3,3,3,3,3,3,3,3,3,3,3,3,3,3,3,4),(1.273268146625E-9,0.000305183030965793,
0.000618697405662781,0.000865973237167115,0.000907586176443213,0.0014325817358511,
0.00178321767141051,0.00181517235288642,0.002336792376541,0.00270521777421962,
0.00272275852932964,0.0031677449805063,0.00317655161755125,0.00351188757997544,
0.00363034470577286,0.00363091529585842,0.00404743389236458,0.00446889752799985,
0.00453793088221608,0.00455651100281012,0.005120350539528,0.0054455170586593,
0.00547872254023126,0.00584209036187464,0.00622546925983902,0.00635310323510253,
0.00664528416314504,0.00695298625517104,0.00726068834719704),
 .UNSPECIFIED.);
#699=B_SPLINE_CURVE_WITH_KNOTS('',3,(#29263,#29264,#29265,#29266,#29267,
#29268,#29269,#29270,#29271,#29272,#29273,#29274,#29275,#29276,#29277,#29278,
#29279,#29280),.UNSPECIFIED.,.F.,.F.,(4,2,2,2,2,2,2,2,4),(0.,0.0707692450882043,
0.141538490176409,0.212305911681142,0.283073333185875,0.353840754690609,
0.424608176195343,0.495377421283547,0.566146666371752),.UNSPECIFIED.);
#700=B_SPLINE_CURVE_WITH_KNOTS('',3,(#29281,#29282,#29283,#29284,#29285,
#29286,#29287,#29288,#29289,#29290,#29291,#29292,#29293,#29294,#29295,#29296,
#29297,#29298),.UNSPECIFIED.,.F.,.F.,(4,2,2,2,2,2,2,2,4),(0.566146666371752,
0.636915911459956,0.70768515654816,0.778452578052894,0.849219999557628,
0.919987421062361,0.990754842567095,1.0615240876553,1.1322933327435),
 .UNSPECIFIED.);
#701=B_SPLINE_CURVE_WITH_KNOTS('',3,(#29301,#29302,#29303,#29304,#29305,
#29306,#29307,#29308,#29309,#29310,#29311,#29312,#29313,#29314,#29315,#29316,
#29317,#29318),.UNSPECIFIED.,.F.,.F.,(4,2,2,2,2,2,2,2,4),(0.,0.0707692450882054,
0.141538490176411,0.212305911681144,0.283073333185877,0.35384075469061,
0.424608176195344,0.495377421283548,0.566146666371752),.UNSPECIFIED.);
#702=B_SPLINE_CURVE_WITH_KNOTS('',3,(#29319,#29320,#29321,#29322,#29323,
#29324,#29325,#29326,#29327,#29328,#29329,#29330,#29331,#29332,#29333,#29334,
#29335,#29336),.UNSPECIFIED.,.F.,.F.,(4,2,2,2,2,2,2,2,4),(0.566146666371752,
0.636915911459956,0.70768515654816,0.778452578052894,0.849219999557627,
0.91998742106236,0.990754842567093,1.0615240876553,1.1322933327435),
 .UNSPECIFIED.);
#703=B_SPLINE_CURVE_WITH_KNOTS('',3,(#29339,#29340,#29341,#29342,#29343,
#29344,#29345,#29346,#29347,#29348,#29349,#29350,#29351,#29352,#29353,#29354,
#29355,#29356),.UNSPECIFIED.,.F.,.F.,(4,2,2,2,2,2,2,2,4),(0.,0.0707692450882044,
0.141538490176409,0.212305911681142,0.283073333185876,0.353840754690609,
0.424608176195343,0.495377421283547,0.566146666371752),.UNSPECIFIED.);
#704=B_SPLINE_CURVE_WITH_KNOTS('',3,(#29357,#29358,#29359,#29360,#29361,
#29362,#29363,#29364,#29365,#29366,#29367,#29368,#29369,#29370,#29371,#29372,
#29373,#29374),.UNSPECIFIED.,.F.,.F.,(4,2,2,2,2,2,2,2,4),(0.566146666371752,
0.636915911459956,0.707685156548161,0.778452578052894,0.849219999557628,
0.919987421062361,0.990754842567095,1.0615240876553,1.1322933327435),
 .UNSPECIFIED.);
#705=B_SPLINE_CURVE_WITH_KNOTS('',3,(#29377,#29378,#29379,#29380,#29381,
#29382,#29383,#29384,#29385,#29386,#29387,#29388,#29389,#29390,#29391,#29392,
#29393,#29394),.UNSPECIFIED.,.F.,.F.,(4,2,2,2,2,2,2,2,4),(0.,0.0707692450882054,
0.141538490176411,0.212305911681144,0.283073333185877,0.353840754690611,
0.424608176195344,0.495377421283549,0.566146666371754),.UNSPECIFIED.);
#706=B_SPLINE_CURVE_WITH_KNOTS('',3,(#29395,#29396,#29397,#29398,#29399,
#29400,#29401,#29402,#29403,#29404,#29405,#29406,#29407,#29408,#29409,#29410,
#29411,#29412),.UNSPECIFIED.,.F.,.F.,(4,2,2,2,2,2,2,2,4),(0.566146666371754,
0.63691591145996,0.707685156548165,0.778452578052898,0.849219999557631,
0.919987421062365,0.990754842567098,1.0615240876553,1.13229333274351),
 .UNSPECIFIED.);
#707=B_SPLINE_CURVE_WITH_KNOTS('',3,(#29415,#29416,#29417,#29418,#29419,
#29420,#29421,#29422,#29423,#29424,#29425,#29426,#29427,#29428,#29429,#29430,
#29431,#29432,#29433),.UNSPECIFIED.,.F.,.F.,(4,2,2,2,3,2,2,2,4),(0.849219999557622,
0.919987421062355,0.990754842567088,1.06152408765529,1.1322933327435,1.2030625778317,
1.27383182291991,1.34459924442464,1.41536666592937),.UNSPECIFIED.);
#708=B_SPLINE_CURVE_WITH_KNOTS('',3,(#29434,#29435,#29436,#29437,#29438,
#29439,#29440,#29441,#29442,#29443,#29444,#29445,#29446,#29447,#29448,#29449,
#29450,#29451),.UNSPECIFIED.,.F.,.F.,(4,2,2,2,2,2,2,2,4),(1.41536666592937,
1.4861340874341,1.55690150893884,1.62767075402704,1.69843999911525,1.76920924420345,
1.83997848929165,1.91074591079639,1.98151333230112),.UNSPECIFIED.);
#709=B_SPLINE_CURVE_WITH_KNOTS('',3,(#29484,#29485,#29486,#29487,#29488,
#29489,#29490,#29491,#29492,#29493,#29494,#29495,#29496,#29497,#29498,#29499,
#29500,#29501),.UNSPECIFIED.,.F.,.F.,(4,2,2,2,2,2,2,2,4),(4.77682283355534E-9,
0.00075938273231847,0.00151876546463694,0.00227814819695541,0.00303753092927388,
0.00379691366159235,0.00455629639391082,0.00531567912622929,0.00607506185854776),
 .UNSPECIFIED.);
#710=B_SPLINE_CURVE_WITH_KNOTS('',3,(#29510,#29511,#29512,#29513,#29514,
#29515,#29516,#29517,#29518,#29519,#29520,#29521,#29522,#29523,#29524,#29525,
#29526,#29527,#29528,#29529,#29530,#29531,#29532,#29533,#29534,#29535,#29536,
#29537,#29538,#29539,#29540,#29541,#29542,#29543,#29544,#29545,#29546,#29547,
#29548,#29549,#29550,#29551,#29552,#29553,#29554,#29555,#29556,#29557,#29558,
#29559,#29560,#29561,#29562,#29563,#29564,#29565,#29566,#29567,#29568,#29569,
#29570,#29571,#29572,#29573,#29574,#29575,#29576,#29577,#29578,#29579,#29580,
#29581,#29582,#29583,#29584,#29585,#29586,#29587,#29588,#29589,#29590,#29591),
 .UNSPECIFIED.,.F.,.F.,(4,3,3,3,3,3,3,3,3,3,3,3,3,3,3,3,3,3,3,3,3,3,3,3,
3,3,3,4),(0.,0.0004211704095861,0.000817473654555697,0.00118439929991323,
0.00140274866617539,0.00152429215349839,0.00189673183671225,0.00222892904096502,
0.00228643823024759,0.00259994712936789,0.00290784220121708,0.00304730469033869,
0.00304858430699679,0.00332638406781091,0.00345576304453128,0.00374859930974991,
0.00381073038374598,0.00386547246148279,0.00412567953064968,0.00419180342212058,
0.00453614859577863,0.00457287646049518,0.00469199913147008,0.0050854186274231,
0.00533502253724438,0.00552937120160224,0.00586539666303883,0.00609716861399357),
 .UNSPECIFIED.);
#711=B_SPLINE_CURVE_WITH_KNOTS('',3,(#29600,#29601,#29602,#29603,#29604,
#29605,#29606,#29607,#29608,#29609,#29610,#29611,#29612,#29613,#29614,#29615,
#29616,#29617),.UNSPECIFIED.,.F.,.F.,(4,2,2,2,2,2,2,2,4),(4.77682273112898E-9,
0.00075938273231847,0.00151876546463694,0.00227814819695541,0.00303753092927388,
0.00379691366159235,0.00455629639391082,0.00531567912622929,0.00607506185854776),
 .UNSPECIFIED.);
#712=B_SPLINE_CURVE_WITH_KNOTS('',3,(#29626,#29627,#29628,#29629,#29630,
#29631,#29632,#29633,#29634,#29635,#29636,#29637,#29638,#29639,#29640,#29641,
#29642,#29643,#29644,#29645,#29646,#29647,#29648,#29649,#29650,#29651,#29652,
#29653,#29654,#29655,#29656,#29657,#29658,#29659,#29660,#29661,#29662,#29663,
#29664,#29665,#29666,#29667,#29668,#29669,#29670,#29671,#29672,#29673,#29674,
#29675,#29676,#29677,#29678,#29679,#29680,#29681,#29682,#29683,#29684,#29685,
#29686,#29687,#29688,#29689,#29690,#29691,#29692,#29693,#29694,#29695,#29696,
#29697,#29698,#29699,#29700,#29701,#29702,#29703,#29704,#29705,#29706,#29707,
#29708,#29709,#29710),.UNSPECIFIED.,.F.,.F.,(4,3,3,3,3,3,3,3,3,3,3,3,3,
3,3,3,3,3,3,3,3,3,3,3,3,3,3,3,4),(0.,0.000450053972194884,0.00056431495950664,
0.000759601302696842,0.00117337414957987,0.001397743801198,0.00151920260539368,
0.00184099933344668,0.00214827687898448,0.00222197528808396,0.00227880390809053,
0.00263007039899105,0.00303752617006762,0.00303840521078737,0.00331462895684914,
0.00344451241700138,0.00373559439233855,0.00379800651348421,0.00385273052115206,
0.00411271653974196,0.00417780716483263,0.00451675956026997,0.00455760781618105,
0.004676243259529,0.00506171900842959,0.0053172091188779,0.00551058612136977,
0.00584478941941549,0.00607681042157474),.UNSPECIFIED.);
#713=B_SPLINE_CURVE_WITH_KNOTS('',3,(#29719,#29720,#29721,#29722,#29723,
#29724,#29725,#29726,#29727,#29728,#29729,#29730,#29731,#29732,#29733,#29734,
#29735,#29736,#29737,#29738,#29739,#29740,#29741,#29742,#29743,#29744,#29745,
#29746,#29747,#29748,#29749,#29750,#29751,#29752,#29753,#29754,#29755,#29756,
#29757,#29758,#29759,#29760,#29761,#29762,#29763,#29764,#29765,#29766,#29767,
#29768,#29769,#29770,#29771,#29772,#29773,#29774,#29775,#29776,#29777,#29778,
#29779,#29780,#29781,#29782,#29783,#29784,#29785,#29786,#29787,#29788,#29789,
#29790,#29791,#29792,#29793,#29794,#29795,#29796,#29797,#29798,#29799,#29800),
 .UNSPECIFIED.,.F.,.F.,(4,3,3,3,3,3,3,3,3,3,3,3,3,3,3,3,3,3,3,3,3,3,3,3,
3,3,3,4),(0.,0.000421170409560706,0.000817473654507556,0.00118439929984293,
0.00140274866617529,0.00152429215349839,0.00189673183664917,0.00222892904096503,
0.00228643823024759,0.00259994712938916,0.00290784220125873,0.00304730469033868,
0.00304858430699679,0.0033263840678449,0.00345576304453138,0.00374859930978851,
0.00381073038374598,0.00386547246148282,0.00412567953064846,0.00419180342212058,
0.00453614859565633,0.00457287646049518,0.00469199913147023,0.00508541862720809,
0.00533502253724438,0.00552937120160261,0.00586539666311319,0.00609716861399357),
 .UNSPECIFIED.);
#714=B_SPLINE_CURVE_WITH_KNOTS('',3,(#29804,#29805,#29806,#29807,#29808,
#29809,#29810,#29811,#29812,#29813,#29814,#29815,#29816,#29817,#29818,#29819,
#29820,#29821),.UNSPECIFIED.,.F.,.F.,(4,2,2,2,2,2,2,2,4),(4.77682281082537E-9,
0.000759382732318467,0.00151876546463693,0.0022781481969554,0.00303753092927387,
0.00379691366159234,0.0045562963939108,0.00531567912622927,0.00607506185854774),
 .UNSPECIFIED.);
#715=B_SPLINE_CURVE_WITH_KNOTS('',3,(#29835,#29836,#29837,#29838,#29839,
#29840,#29841,#29842,#29843,#29844,#29845,#29846,#29847,#29848,#29849,#29850,
#29851,#29852,#29853,#29854,#29855,#29856,#29857,#29858,#29859,#29860,#29861,
#29862,#29863,#29864,#29865,#29866,#29867,#29868,#29869,#29870,#29871,#29872,
#29873,#29874,#29875,#29876,#29877,#29878,#29879,#29880,#29881,#29882,#29883,
#29884,#29885,#29886,#29887,#29888,#29889,#29890,#29891,#29892,#29893,#29894,
#29895,#29896,#29897,#29898,#29899,#29900,#29901,#29902,#29903,#29904,#29905,
#29906,#29907,#29908,#29909,#29910,#29911,#29912,#29913,#29914,#29915,#29916),
 .UNSPECIFIED.,.F.,.F.,(4,3,3,3,3,3,3,3,3,3,3,3,3,3,3,3,3,3,3,3,3,3,3,3,
3,3,3,4),(0.,0.00042117040958297,0.000817473654550321,0.00118439929990684,
0.00140274866617551,0.00152429215349839,0.00189673183686581,0.00222892904096507,
0.00228643823024759,0.00259994712942609,0.00290784220133854,0.00304730469033868,
0.00304858430699679,0.00332638406787497,0.00345576304453135,0.00374859930981913,
0.00381073038374599,0.00386547246148282,0.00412567953059812,0.00419180342212059,
0.00453614859568482,0.00457287646049519,0.00469199913147008,0.00508541862749306,
0.00533502253724438,0.00552937120160218,0.00586539666303646,0.00609716861399358),
 .UNSPECIFIED.);
#716=B_SPLINE_CURVE_WITH_KNOTS('',3,(#29925,#29926,#29927,#29928,#29929,
#29930,#29931,#29932,#29933,#29934,#29935,#29936,#29937,#29938,#29939,#29940,
#29941,#29942),.UNSPECIFIED.,.F.,.F.,(4,2,2,2,2,2,2,2,4),(4.77682282016954E-9,
0.00075938273231847,0.00151876546463694,0.00227814819695541,0.00303753092927388,
0.00379691366159235,0.00455629639391082,0.00531567912622929,0.00607506185854776),
 .UNSPECIFIED.);
#717=B_SPLINE_CURVE_WITH_KNOTS('',3,(#29951,#29952,#29953,#29954,#29955,
#29956,#29957,#29958,#29959,#29960,#29961,#29962,#29963,#29964,#29965,#29966,
#29967,#29968,#29969,#29970,#29971,#29972,#29973,#29974,#29975,#29976,#29977,
#29978,#29979,#29980,#29981,#29982,#29983,#29984,#29985,#29986,#29987,#29988,
#29989,#29990,#29991,#29992,#29993,#29994,#29995,#29996,#29997,#29998,#29999,
#30000,#30001,#30002,#30003,#30004,#30005,#30006,#30007,#30008,#30009,#30010,
#30011,#30012,#30013,#30014,#30015,#30016,#30017,#30018,#30019,#30020,#30021,
#30022,#30023,#30024,#30025,#30026,#30027,#30028,#30029,#30030,#30031,#30032,
#30033,#30034,#30035),.UNSPECIFIED.,.F.,.F.,(4,3,3,3,3,3,3,3,3,3,3,3,3,
3,3,3,3,3,3,3,3,3,3,3,3,3,3,3,4),(0.,0.000450053972178455,0.000564314959506638,
0.000759601302696842,0.00117337414953125,0.001397743801198,0.00151920260539368,
0.00184099933344431,0.00214827687897479,0.0022219752880839,0.00227880390809053,
0.00263007039899095,0.00303752617006762,0.00303840521078737,0.00331462895687695,
0.00344451241700149,0.00373559439236671,0.00379800651348421,0.00385273052115206,
0.00411271653966241,0.00417780716483263,0.00451675956044004,0.00455760781618105,
0.00467624325952877,0.00506171900826484,0.0053172091188779,0.00551058612137,
0.00584478941937396,0.00607681042157474),.UNSPECIFIED.);
#718=B_SPLINE_CURVE_WITH_KNOTS('',3,(#30044,#30045,#30046,#30047,#30048,
#30049,#30050,#30051,#30052,#30053,#30054,#30055,#30056,#30057,#30058,#30059,
#30060,#30061,#30062,#30063,#30064,#30065,#30066,#30067,#30068,#30069,#30070,
#30071,#30072,#30073,#30074,#30075,#30076,#30077,#30078,#30079,#30080,#30081,
#30082,#30083,#30084,#30085,#30086,#30087,#30088,#30089,#30090,#30091,#30092,
#30093,#30094,#30095,#30096,#30097,#30098,#30099,#30100,#30101,#30102,#30103,
#30104,#30105,#30106,#30107,#30108,#30109,#30110,#30111,#30112,#30113,#30114,
#30115,#30116,#30117,#30118,#30119,#30120,#30121,#30122,#30123,#30124,#30125),
 .UNSPECIFIED.,.F.,.F.,(4,3,3,3,3,3,3,3,3,3,3,3,3,3,3,3,3,3,3,3,3,3,3,3,
3,3,3,4),(0.,0.000421170409563676,0.000817473654515121,0.00118439929985521,
0.0014027486661753,0.0015242921534984,0.00189673183663668,0.00222892904096502,
0.0022864382302476,0.00259994712935677,0.00290784220118465,0.00304730469033869,
0.0030485843069968,0.0033263840678324,0.00345576304453135,0.00374859930976709,
0.003810730383746,0.00386547246148282,0.00412567953061791,0.00419180342212059,
0.00453614859574039,0.00457287646049519,0.00469199913147009,0.00508541862740153,
0.00533502253724439,0.00552937120160227,0.0058653966630742,0.00609716861399359),
 .UNSPECIFIED.);
#719=B_SPLINE_CURVE_WITH_KNOTS('',3,(#30192,#30193,#30194,#30195,#30196,
#30197,#30198,#30199,#30200,#30201,#30202,#30203,#30204,#30205,#30206,#30207),
 .UNSPECIFIED.,.F.,.F.,(4,3,3,3,3,4),(-4.96552337022927E-6,0.00010764588910917,
0.000210094846213861,0.000303745134247416,0.000388498757831818,0.000430337104598325),
 .UNSPECIFIED.);
#720=B_SPLINE_CURVE_WITH_KNOTS('',3,(#30210,#30211,#30212,#30213,#30214,
#30215,#30216,#30217),.UNSPECIFIED.,.F.,.F.,(4,2,2,4),(-0.000433447002133302,
0.,0.0387852866187773,0.0560629149274059),.UNSPECIFIED.);
#721=B_SPLINE_CURVE_WITH_KNOTS('',3,(#30219,#30220,#30221,#30222,#30223,
#30224,#30225,#30226),.UNSPECIFIED.,.F.,.F.,(4,2,2,4),(0.137724521771023,
0.151853084795163,0.183569264620213,0.183923710449112),.UNSPECIFIED.);
#722=B_SPLINE_CURVE_WITH_KNOTS('',3,(#30294,#30295,#30296,#30297,#30298,
#30299,#30300,#30301,#30302,#30303,#30304,#30305,#30306,#30307,#30308,#30309),
 .UNSPECIFIED.,.F.,.F.,(4,3,3,3,3,4),(-4.96552472797221E-6,0.000107645888232349,
0.00021009484556578,0.000303745133732349,0.000388498757401816,0.000430337104597686),
 .UNSPECIFIED.);
#723=B_SPLINE_CURVE_WITH_KNOTS('',3,(#30312,#30313,#30314,#30315,#30316,
#30317,#30318,#30319),.UNSPECIFIED.,.F.,.F.,(4,2,2,4),(-0.000433447001819931,
0.,0.0387852865238832,0.0560629147500476),.UNSPECIFIED.);
#724=B_SPLINE_CURVE_WITH_KNOTS('',3,(#30321,#30322,#30323,#30324,#30325,
#30326,#30327,#30328),.UNSPECIFIED.,.F.,.F.,(4,2,2,4),(0.137724521771001,
0.151853084794259,0.183569264683853,0.183923710514055),.UNSPECIFIED.);
#725=B_SPLINE_CURVE_WITH_KNOTS('',3,(#30384,#30385,#30386,#30387,#30388,
#30389,#30390,#30391,#30392,#30393,#30394,#30395,#30396,#30397,#30398,#30399),
 .UNSPECIFIED.,.F.,.F.,(4,3,3,3,3,4),(-4.9655233990862E-6,0.000107645889303446,
0.000210094846471236,0.000303745134532124,0.000388498758142231,0.000430337104598325),
 .UNSPECIFIED.);
#726=B_SPLINE_CURVE_WITH_KNOTS('',3,(#30400,#30401,#30402,#30403,#30404,
#30405,#30406,#30407,#30408,#30409,#30410,#30411,#30412,#30413,#30414,#30415),
 .UNSPECIFIED.,.F.,.F.,(4,3,3,3,3,4),(0.,8.57266868340804E-5,0.00017997859326195,
0.000281094481442682,0.000399483842647333,0.000429651352273076),
 .UNSPECIFIED.);
#727=B_SPLINE_CURVE_WITH_KNOTS('',3,(#30417,#30418,#30419,#30420,#30421,
#30422,#30423,#30424),.UNSPECIFIED.,.F.,.F.,(4,2,2,4),(-0.000433447002036394,
3.69027725044546E-14,0.0387852865738777,0.0560629148434446),
 .UNSPECIFIED.);
#728=B_SPLINE_CURVE_WITH_KNOTS('',3,(#30426,#30427,#30428,#30429,#30430,
#30431,#30432,#30433),.UNSPECIFIED.,.F.,.F.,(4,2,2,4),(0.137724521770918,
0.151853084794576,0.183569264655288,0.183923710484895),.UNSPECIFIED.);
#729=B_SPLINE_CURVE_WITH_KNOTS('',3,(#30501,#30502,#30503,#30504,#30505,
#30506,#30507,#30508,#30509,#30510,#30511,#30512,#30513,#30514,#30515,#30516),
 .UNSPECIFIED.,.F.,.F.,(4,3,3,3,3,4),(-4.96552472794879E-6,0.000107645887808995,
0.000210094845026632,0.00030374513314452,0.000388498756766525,0.000430337104597696),
 .UNSPECIFIED.);
#730=B_SPLINE_CURVE_WITH_KNOTS('',3,(#30519,#30520,#30521,#30522,#30523,
#30524,#30525,#30526),.UNSPECIFIED.,.F.,.F.,(4,2,2,4),(-0.000433447002159874,
0.,0.0387852866200758,0.0560629149297987),.UNSPECIFIED.);
#731=B_SPLINE_CURVE_WITH_KNOTS('',3,(#30528,#30529,#30530,#30531,#30532,
#30533,#30534,#30535),.UNSPECIFIED.,.F.,.F.,(4,2,2,4),(0.137724521771109,
0.151853084795218,0.183569264621138,0.183923710450037),.UNSPECIFIED.);
#732=B_SPLINE_CURVE_WITH_KNOTS('',3,(#30591,#30592,#30593,#30594,#30595,
#30596,#30597,#30598,#30599,#30600,#30601,#30602,#30603,#30604,#30605,#30606),
 .UNSPECIFIED.,.F.,.F.,(4,3,3,3,3,4),(-4.9655233990868E-6,0.000107645889377711,
0.000210094846565806,0.000303745134635254,0.000388498758253666,0.000430337104598325),
 .UNSPECIFIED.);
#733=B_SPLINE_CURVE_WITH_KNOTS('',3,(#30607,#30608,#30609,#30610,#30611,
#30612,#30613,#30614,#30615,#30616,#30617,#30618,#30619,#30620,#30621,#30622),
 .UNSPECIFIED.,.F.,.F.,(4,3,3,3,3,4),(8.67361737988404E-19,8.57266868355843E-5,
0.000179978593251411,0.000281094481402461,0.00039948384249144,0.000429651352272726),
 .UNSPECIFIED.);
#734=B_SPLINE_CURVE_WITH_KNOTS('',3,(#30624,#30625,#30626,#30627,#30628,
#30629,#30630,#30631),.UNSPECIFIED.,.F.,.F.,(4,2,2,4),(-0.000433447001866445,
0.,0.0387852865654643,0.0560629148277019),.UNSPECIFIED.);
#735=B_SPLINE_CURVE_WITH_KNOTS('',3,(#30633,#30634,#30635,#30636,#30637,
#30638,#30639,#30640),.UNSPECIFIED.,.F.,.F.,(4,2,2,4),(0.13772452177113,
0.151853084794678,0.183569264665514,0.183923710495293),.UNSPECIFIED.);
#736=B_SPLINE_CURVE_WITH_KNOTS('',3,(#30708,#30709,#30710,#30711,#30712,
#30713,#30714,#30715,#30716,#30717,#30718,#30719,#30720,#30721,#30722,#30723),
 .UNSPECIFIED.,.F.,.F.,(4,3,3,3,3,4),(-4.9655233702401E-6,0.000107645889063516,
0.000210094846155721,0.000303745134184041,0.000388498757763316,0.000430337104598318),
 .UNSPECIFIED.);
#737=B_SPLINE_CURVE_WITH_KNOTS('',3,(#30726,#30727,#30728,#30729,#30730,
#30731,#30732,#30733),.UNSPECIFIED.,.F.,.F.,(4,2,2,4),(-0.00043344700214138,
0.,0.0387852866057272,0.0560629149029756),.UNSPECIFIED.);
#738=B_SPLINE_CURVE_WITH_KNOTS('',3,(#30735,#30736,#30737,#30738,#30739,
#30740,#30741,#30742),.UNSPECIFIED.,.F.,.F.,(4,2,2,4),(0.137724521771185,
0.151853084795333,0.183569264617388,0.183923710446234),.UNSPECIFIED.);
#739=B_SPLINE_CURVE_WITH_KNOTS('',3,(#30810,#30811,#30812,#30813,#30814,
#30815,#30816,#30817,#30818,#30819,#30820,#30821,#30822,#30823,#30824,#30825),
 .UNSPECIFIED.,.F.,.F.,(4,3,3,3,3,4),(-4.96552472796978E-6,0.000107645888261097,
0.000210094845602384,0.000303745133772396,0.000388498757445142,0.000430337104597697),
 .UNSPECIFIED.);
#740=B_SPLINE_CURVE_WITH_KNOTS('',3,(#30828,#30829,#30830,#30831,#30832,
#30833,#30834,#30835),.UNSPECIFIED.,.F.,.F.,(4,2,2,4),(-0.00043344700187696,
0.,0.0387852865361233,0.0560629147728757),.UNSPECIFIED.);
#741=B_SPLINE_CURVE_WITH_KNOTS('',3,(#30837,#30838,#30839,#30840,#30841,
#30842,#30843,#30844),.UNSPECIFIED.,.F.,.F.,(4,2,2,4),(0.137724521771103,
0.151853084794522,0.183569264674518,0.183923710504536),.UNSPECIFIED.);
#742=B_SPLINE_CURVE_WITH_KNOTS('',3,(#30900,#30901,#30902,#30903,#30904,
#30905,#30906,#30907,#30908,#30909,#30910,#30911,#30912,#30913,#30914,#30915),
 .UNSPECIFIED.,.F.,.F.,(4,3,3,3,3,4),(-4.96552339908152E-6,0.000107645889444403,
0.000210094846650772,0.000303745134727905,0.000388498758353848,0.000430337104598325),
 .UNSPECIFIED.);
#743=B_SPLINE_CURVE_WITH_KNOTS('',3,(#30916,#30917,#30918,#30919,#30920,
#30921,#30922,#30923,#30924,#30925,#30926,#30927,#30928,#30929,#30930,#30931),
 .UNSPECIFIED.,.F.,.F.,(4,3,3,3,3,4),(4.33680868994202E-19,8.57266868349673E-5,
0.000179978593250927,0.000281094481403179,0.000399483842498987,0.000429651352273256),
 .UNSPECIFIED.);
#744=B_SPLINE_CURVE_WITH_KNOTS('',3,(#30933,#30934,#30935,#30936,#30937,
#30938,#30939,#30940),.UNSPECIFIED.,.F.,.F.,(4,2,2,4),(-0.00043344700190692,
0.,0.0387852865487993,0.0560629147965774),.UNSPECIFIED.);
#745=B_SPLINE_CURVE_WITH_KNOTS('',3,(#30942,#30943,#30944,#30945,#30946,
#30947,#30948,#30949),.UNSPECIFIED.,.F.,.F.,(4,2,2,4),(0.137724521770992,
0.151853084794507,0.183569264670678,0.183923710500586),.UNSPECIFIED.);
#746=B_SPLINE_CURVE_WITH_KNOTS('',3,(#31017,#31018,#31019,#31020,#31021,
#31022,#31023,#31024,#31025,#31026,#31027,#31028,#31029,#31030,#31031,#31032),
 .UNSPECIFIED.,.F.,.F.,(4,3,3,3,3,4),(-4.96552472798547E-6,0.000107645888160522,
0.000210094845474309,0.000303745133632723,0.000388498757294183,0.000430337104597689),
 .UNSPECIFIED.);
#747=B_SPLINE_CURVE_WITH_KNOTS('',3,(#31035,#31036,#31037,#31038,#31039,
#31040,#31041,#31042),.UNSPECIFIED.,.F.,.F.,(4,2,2,4),(-0.000433447001961007,
0.,0.0387852865485228,0.0560629147960515),.UNSPECIFIED.);
#748=B_SPLINE_CURVE_WITH_KNOTS('',3,(#31044,#31045,#31046,#31047,#31048,
#31049,#31050,#31051),.UNSPECIFIED.,.F.,.F.,(4,2,2,4),(0.137724521771081,
0.151853084794498,0.183569264679235,0.183923710509208),.UNSPECIFIED.);
#749=B_SPLINE_CURVE_WITH_KNOTS('',3,(#31107,#31108,#31109,#31110,#31111,
#31112,#31113,#31114,#31115,#31116,#31117,#31118,#31119,#31120,#31121,#31122),
 .UNSPECIFIED.,.F.,.F.,(4,3,3,3,3,4),(-4.96552339908991E-6,0.000107645889258478,
0.000210094846413965,0.000303745134469702,0.00038849875807473,0.000430337104598321),
 .UNSPECIFIED.);
#750=B_SPLINE_CURVE_WITH_KNOTS('',3,(#31123,#31124,#31125,#31126,#31127,
#31128,#31129,#31130,#31131,#31132,#31133,#31134,#31135,#31136,#31137,#31138),
 .UNSPECIFIED.,.F.,.F.,(4,3,3,3,3,4),(4.33680868994202E-19,8.57266868340056E-5,
0.000179978593272076,0.000281094481476539,0.000399483842768878,0.000429651352272027),
 .UNSPECIFIED.);
#751=B_SPLINE_CURVE_WITH_KNOTS('',3,(#31140,#31141,#31142,#31143,#31144,
#31145,#31146,#31147),.UNSPECIFIED.,.F.,.F.,(4,2,2,4),(-0.000433447002021717,
0.,0.0387852865801805,0.0560629148552472),.UNSPECIFIED.);
#752=B_SPLINE_CURVE_WITH_KNOTS('',3,(#31149,#31150,#31151,#31152,#31153,
#31154,#31155,#31156),.UNSPECIFIED.,.F.,.F.,(4,2,2,4),(0.137724521771083,
0.151853084794822,0.183569264651922,0.183923710481445),.UNSPECIFIED.);
#753=PLANE('',#10389);
#754=PLANE('',#10390);
#755=PLANE('',#10391);
#756=PLANE('',#10392);
#757=PLANE('',#10393);
#758=PLANE('',#10394);
#759=PLANE('',#10395);
#760=PLANE('',#10396);
#761=PLANE('',#10397);
#762=PLANE('',#10398);
#763=PLANE('',#10399);
#764=PLANE('',#10400);
#765=PLANE('',#10401);
#766=PLANE('',#10402);
#767=PLANE('',#10403);
#768=PLANE('',#10404);
#769=PLANE('',#10405);
#770=PLANE('',#10406);
#771=PLANE('',#10407);
#772=PLANE('',#10408);
#773=PLANE('',#10409);
#774=PLANE('',#10410);
#775=PLANE('',#10411);
#776=PLANE('',#10412);
#777=PLANE('',#10413);
#778=PLANE('',#10414);
#779=PLANE('',#10415);
#780=PLANE('',#10416);
#781=PLANE('',#10417);
#782=PLANE('',#10418);
#783=PLANE('',#10419);
#784=PLANE('',#10420);
#785=PLANE('',#10421);
#786=PLANE('',#10422);
#787=PLANE('',#10423);
#788=PLANE('',#10424);
#789=PLANE('',#10425);
#790=PLANE('',#10426);
#791=PLANE('',#10427);
#792=PLANE('',#10428);
#793=PLANE('',#10429);
#794=PLANE('',#10430);
#795=PLANE('',#10431);
#796=PLANE('',#10432);
#797=PLANE('',#10433);
#798=PLANE('',#10434);
#799=PLANE('',#10435);
#800=PLANE('',#10436);
#801=PLANE('',#10437);
#802=PLANE('',#10438);
#803=PLANE('',#10439);
#804=PLANE('',#10440);
#805=PLANE('',#10441);
#806=PLANE('',#10442);
#807=PLANE('',#10443);
#808=PLANE('',#10444);
#809=PLANE('',#10445);
#810=PLANE('',#10446);
#811=PLANE('',#10447);
#812=PLANE('',#10448);
#813=PLANE('',#10449);
#814=PLANE('',#10450);
#815=PLANE('',#10451);
#816=PLANE('',#10452);
#817=PLANE('',#10453);
#818=PLANE('',#10454);
#819=PLANE('',#10455);
#820=PLANE('',#10456);
#821=PLANE('',#10457);
#822=PLANE('',#10458);
#823=PLANE('',#10459);
#824=PLANE('',#10460);
#825=PLANE('',#10461);
#826=PLANE('',#10462);
#827=PLANE('',#10463);
#828=PLANE('',#10464);
#829=PLANE('',#10465);
#830=PLANE('',#10466);
#831=PLANE('',#10467);
#832=PLANE('',#10468);
#833=PLANE('',#10472);
#834=PLANE('',#10474);
#835=PLANE('',#10489);
#836=PLANE('',#10500);
#837=PLANE('',#10512);
#838=PLANE('',#10513);
#839=PLANE('',#10514);
#840=PLANE('',#10515);
#841=PLANE('',#10516);
#842=PLANE('',#10517);
#843=PLANE('',#10520);
#844=PLANE('',#10521);
#845=PLANE('',#10522);
#846=PLANE('',#10523);
#847=PLANE('',#10524);
#848=PLANE('',#10525);
#849=PLANE('',#10526);
#850=PLANE('',#10528);
#851=PLANE('',#10534);
#852=PLANE('',#10540);
#853=PLANE('',#10544);
#854=PLANE('',#10547);
#855=PLANE('',#10552);
#856=PLANE('',#10553);
#857=PLANE('',#10563);
#858=PLANE('',#10564);
#859=PLANE('',#10566);
#860=PLANE('',#10567);
#861=PLANE('',#10568);
#862=PLANE('',#10569);
#863=PLANE('',#10574);
#864=PLANE('',#10577);
#865=PLANE('',#10587);
#866=PLANE('',#10588);
#867=PLANE('',#10589);
#868=PLANE('',#10591);
#869=PLANE('',#10597);
#870=PLANE('',#10598);
#871=PLANE('',#10599);
#872=PLANE('',#10600);
#873=PLANE('',#10601);
#874=PLANE('',#10602);
#875=PLANE('',#10603);
#876=PLANE('',#10604);
#877=PLANE('',#10605);
#878=PLANE('',#10606);
#879=PLANE('',#10607);
#880=PLANE('',#10608);
#881=PLANE('',#10609);
#882=PLANE('',#10610);
#883=PLANE('',#10611);
#884=PLANE('',#10612);
#885=PLANE('',#10620);
#886=PLANE('',#10622);
#887=PLANE('',#10627);
#888=PLANE('',#10633);
#889=PLANE('',#10639);
#890=PLANE('',#10648);
#891=PLANE('',#10651);
#892=PLANE('',#10652);
#893=PLANE('',#10659);
#894=PLANE('',#10675);
#895=PLANE('',#10676);
#896=PLANE('',#10686);
#897=PLANE('',#10687);
#898=PLANE('',#10715);
#899=PLANE('',#10718);
#900=PLANE('',#10771);
#901=PLANE('',#10773);
#902=PLANE('',#10777);
#903=PLANE('',#10780);
#904=PLANE('',#10783);
#905=PLANE('',#10788);
#906=PLANE('',#10799);
#907=PLANE('',#10800);
#908=PLANE('',#10801);
#909=PLANE('',#10802);
#910=PLANE('',#10803);
#911=PLANE('',#10804);
#912=PLANE('',#10805);
#913=PLANE('',#10806);
#914=PLANE('',#10808);
#915=PLANE('',#10810);
#916=PLANE('',#10812);
#917=PLANE('',#10813);
#918=PLANE('',#10819);
#919=PLANE('',#10821);
#920=PLANE('',#10826);
#921=PLANE('',#10827);
#922=PLANE('',#10828);
#923=PLANE('',#10829);
#924=PLANE('',#10830);
#925=PLANE('',#10831);
#926=PLANE('',#10836);
#927=PLANE('',#10837);
#928=PLANE('',#10838);
#929=PLANE('',#10839);
#930=PLANE('',#10840);
#931=PLANE('',#10841);
#932=PLANE('',#10842);
#933=PLANE('',#10843);
#934=PLANE('',#10844);
#935=PLANE('',#10845);
#936=PLANE('',#10846);
#937=PLANE('',#10847);
#938=PLANE('',#10848);
#939=PLANE('',#10849);
#940=PLANE('',#10850);
#941=PLANE('',#10851);
#942=PLANE('',#10852);
#943=PLANE('',#10853);
#944=PLANE('',#10854);
#945=PLANE('',#10855);
#946=PLANE('',#10856);
#947=PLANE('',#10857);
#948=PLANE('',#10858);
#949=PLANE('',#10859);
#950=PLANE('',#10860);
#951=PLANE('',#10861);
#952=PLANE('',#10862);
#953=PLANE('',#10863);
#954=PLANE('',#10864);
#955=PLANE('',#10865);
#956=PLANE('',#10866);
#957=PLANE('',#10867);
#958=PLANE('',#10873);
#959=PLANE('',#10874);
#960=PLANE('',#10879);
#961=PLANE('',#10880);
#962=PLANE('',#10882);
#963=PLANE('',#10885);
#964=PLANE('',#10908);
#965=PLANE('',#10912);
#966=PLANE('',#10913);
#967=PLANE('',#10918);
#968=PLANE('',#10919);
#969=PLANE('',#10952);
#970=PLANE('',#10973);
#971=PLANE('',#10981);
#972=PLANE('',#10987);
#973=PLANE('',#10998);
#974=PLANE('',#11002);
#975=PLANE('',#11060);
#976=PLANE('',#11063);
#977=PLANE('',#11065);
#978=PLANE('',#11066);
#979=PLANE('',#11067);
#980=PLANE('',#11068);
#981=PLANE('',#11069);
#982=PLANE('',#11070);
#983=PLANE('',#11078);
#984=PLANE('',#11080);
#985=PLANE('',#11081);
#986=PLANE('',#11082);
#987=PLANE('',#11083);
#988=PLANE('',#11084);
#989=PLANE('',#11085);
#990=PLANE('',#11086);
#991=PLANE('',#11087);
#992=PLANE('',#11088);
#993=PLANE('',#11089);
#994=PLANE('',#11090);
#995=PLANE('',#11091);
#996=PLANE('',#11092);
#997=PLANE('',#11093);
#998=PLANE('',#11094);
#999=PLANE('',#11095);
#1000=PLANE('',#11096);
#1001=PLANE('',#11097);
#1002=PLANE('',#11111);
#1003=PLANE('',#11112);
#1004=PLANE('',#11114);
#1005=PLANE('',#11124);
#1006=PLANE('',#11128);
#1007=PLANE('',#11144);
#1008=PLANE('',#11160);
#1009=PLANE('',#11167);
#1010=PLANE('',#11176);
#1011=PLANE('',#11182);
#1012=PLANE('',#11188);
#1013=PLANE('',#11196);
#1014=PLANE('',#11204);
#1015=PLANE('',#11205);
#1016=PLANE('',#11206);
#1017=PLANE('',#11207);
#1018=PLANE('',#11208);
#1019=PLANE('',#11209);
#1020=FACE_OUTER_BOUND('',#1576,.T.);
#1021=FACE_OUTER_BOUND('',#1577,.T.);
#1022=FACE_OUTER_BOUND('',#1578,.T.);
#1023=FACE_OUTER_BOUND('',#1579,.T.);
#1024=FACE_OUTER_BOUND('',#1580,.T.);
#1025=FACE_OUTER_BOUND('',#1581,.T.);
#1026=FACE_OUTER_BOUND('',#1582,.T.);
#1027=FACE_OUTER_BOUND('',#1583,.T.);
#1028=FACE_OUTER_BOUND('',#1584,.T.);
#1029=FACE_OUTER_BOUND('',#1585,.T.);
#1030=FACE_OUTER_BOUND('',#1586,.T.);
#1031=FACE_OUTER_BOUND('',#1587,.T.);
#1032=FACE_OUTER_BOUND('',#1588,.T.);
#1033=FACE_OUTER_BOUND('',#1589,.T.);
#1034=FACE_OUTER_BOUND('',#1590,.T.);
#1035=FACE_OUTER_BOUND('',#1591,.T.);
#1036=FACE_OUTER_BOUND('',#1592,.T.);
#1037=FACE_OUTER_BOUND('',#1593,.T.);
#1038=FACE_OUTER_BOUND('',#1594,.T.);
#1039=FACE_OUTER_BOUND('',#1595,.T.);
#1040=FACE_OUTER_BOUND('',#1596,.T.);
#1041=FACE_OUTER_BOUND('',#1597,.T.);
#1042=FACE_OUTER_BOUND('',#1598,.T.);
#1043=FACE_OUTER_BOUND('',#1599,.T.);
#1044=FACE_OUTER_BOUND('',#1600,.T.);
#1045=FACE_OUTER_BOUND('',#1601,.T.);
#1046=FACE_OUTER_BOUND('',#1602,.T.);
#1047=FACE_OUTER_BOUND('',#1603,.T.);
#1048=FACE_OUTER_BOUND('',#1604,.T.);
#1049=FACE_OUTER_BOUND('',#1605,.T.);
#1050=FACE_OUTER_BOUND('',#1606,.T.);
#1051=FACE_OUTER_BOUND('',#1607,.T.);
#1052=FACE_OUTER_BOUND('',#1608,.T.);
#1053=FACE_OUTER_BOUND('',#1609,.T.);
#1054=FACE_OUTER_BOUND('',#1610,.T.);
#1055=FACE_OUTER_BOUND('',#1611,.T.);
#1056=FACE_OUTER_BOUND('',#1612,.T.);
#1057=FACE_OUTER_BOUND('',#1613,.T.);
#1058=FACE_OUTER_BOUND('',#1614,.T.);
#1059=FACE_OUTER_BOUND('',#1615,.T.);
#1060=FACE_OUTER_BOUND('',#1616,.T.);
#1061=FACE_OUTER_BOUND('',#1617,.T.);
#1062=FACE_OUTER_BOUND('',#1618,.T.);
#1063=FACE_OUTER_BOUND('',#1619,.T.);
#1064=FACE_OUTER_BOUND('',#1620,.T.);
#1065=FACE_OUTER_BOUND('',#1621,.T.);
#1066=FACE_OUTER_BOUND('',#1622,.T.);
#1067=FACE_OUTER_BOUND('',#1623,.T.);
#1068=FACE_OUTER_BOUND('',#1624,.T.);
#1069=FACE_OUTER_BOUND('',#1625,.T.);
#1070=FACE_OUTER_BOUND('',#1626,.T.);
#1071=FACE_OUTER_BOUND('',#1627,.T.);
#1072=FACE_OUTER_BOUND('',#1628,.T.);
#1073=FACE_OUTER_BOUND('',#1629,.T.);
#1074=FACE_OUTER_BOUND('',#1630,.T.);
#1075=FACE_OUTER_BOUND('',#1631,.T.);
#1076=FACE_OUTER_BOUND('',#1632,.T.);
#1077=FACE_OUTER_BOUND('',#1633,.T.);
#1078=FACE_OUTER_BOUND('',#1634,.T.);
#1079=FACE_OUTER_BOUND('',#1635,.T.);
#1080=FACE_OUTER_BOUND('',#1636,.T.);
#1081=FACE_OUTER_BOUND('',#1637,.T.);
#1082=FACE_OUTER_BOUND('',#1638,.T.);
#1083=FACE_OUTER_BOUND('',#1639,.T.);
#1084=FACE_OUTER_BOUND('',#1640,.T.);
#1085=FACE_OUTER_BOUND('',#1641,.T.);
#1086=FACE_OUTER_BOUND('',#1642,.T.);
#1087=FACE_OUTER_BOUND('',#1643,.T.);
#1088=FACE_OUTER_BOUND('',#1644,.T.);
#1089=FACE_OUTER_BOUND('',#1645,.T.);
#1090=FACE_OUTER_BOUND('',#1646,.T.);
#1091=FACE_OUTER_BOUND('',#1647,.T.);
#1092=FACE_OUTER_BOUND('',#1648,.T.);
#1093=FACE_OUTER_BOUND('',#1649,.T.);
#1094=FACE_OUTER_BOUND('',#1650,.T.);
#1095=FACE_OUTER_BOUND('',#1651,.T.);
#1096=FACE_OUTER_BOUND('',#1652,.T.);
#1097=FACE_OUTER_BOUND('',#1653,.T.);
#1098=FACE_OUTER_BOUND('',#1654,.T.);
#1099=FACE_OUTER_BOUND('',#1655,.T.);
#1100=FACE_OUTER_BOUND('',#1656,.T.);
#1101=FACE_OUTER_BOUND('',#1657,.T.);
#1102=FACE_OUTER_BOUND('',#1658,.T.);
#1103=FACE_OUTER_BOUND('',#1659,.T.);
#1104=FACE_OUTER_BOUND('',#1660,.T.);
#1105=FACE_OUTER_BOUND('',#1661,.T.);
#1106=FACE_OUTER_BOUND('',#1662,.T.);
#1107=FACE_OUTER_BOUND('',#1663,.T.);
#1108=FACE_OUTER_BOUND('',#1664,.T.);
#1109=FACE_OUTER_BOUND('',#1665,.T.);
#1110=FACE_OUTER_BOUND('',#1666,.T.);
#1111=FACE_OUTER_BOUND('',#1667,.T.);
#1112=FACE_OUTER_BOUND('',#1668,.T.);
#1113=FACE_OUTER_BOUND('',#1669,.T.);
#1114=FACE_OUTER_BOUND('',#1670,.T.);
#1115=FACE_OUTER_BOUND('',#1671,.T.);
#1116=FACE_OUTER_BOUND('',#1672,.T.);
#1117=FACE_OUTER_BOUND('',#1673,.T.);
#1118=FACE_OUTER_BOUND('',#1674,.T.);
#1119=FACE_OUTER_BOUND('',#1675,.T.);
#1120=FACE_OUTER_BOUND('',#1676,.T.);
#1121=FACE_OUTER_BOUND('',#1677,.T.);
#1122=FACE_OUTER_BOUND('',#1678,.T.);
#1123=FACE_OUTER_BOUND('',#1679,.T.);
#1124=FACE_OUTER_BOUND('',#1680,.T.);
#1125=FACE_OUTER_BOUND('',#1681,.T.);
#1126=FACE_OUTER_BOUND('',#1682,.T.);
#1127=FACE_OUTER_BOUND('',#1683,.T.);
#1128=FACE_OUTER_BOUND('',#1684,.T.);
#1129=FACE_OUTER_BOUND('',#1685,.T.);
#1130=FACE_OUTER_BOUND('',#1686,.T.);
#1131=FACE_OUTER_BOUND('',#1687,.T.);
#1132=FACE_OUTER_BOUND('',#1688,.T.);
#1133=FACE_OUTER_BOUND('',#1689,.T.);
#1134=FACE_OUTER_BOUND('',#1690,.T.);
#1135=FACE_OUTER_BOUND('',#1691,.T.);
#1136=FACE_OUTER_BOUND('',#1692,.T.);
#1137=FACE_OUTER_BOUND('',#1693,.T.);
#1138=FACE_OUTER_BOUND('',#1694,.T.);
#1139=FACE_OUTER_BOUND('',#1695,.T.);
#1140=FACE_OUTER_BOUND('',#1696,.T.);
#1141=FACE_OUTER_BOUND('',#1697,.T.);
#1142=FACE_OUTER_BOUND('',#1699,.T.);
#1143=FACE_OUTER_BOUND('',#1701,.T.);
#1144=FACE_OUTER_BOUND('',#1702,.T.);
#1145=FACE_OUTER_BOUND('',#1703,.T.);
#1146=FACE_OUTER_BOUND('',#1704,.T.);
#1147=FACE_OUTER_BOUND('',#1705,.T.);
#1148=FACE_OUTER_BOUND('',#1706,.T.);
#1149=FACE_OUTER_BOUND('',#1707,.T.);
#1150=FACE_OUTER_BOUND('',#1708,.T.);
#1151=FACE_OUTER_BOUND('',#1709,.T.);
#1152=FACE_OUTER_BOUND('',#1711,.T.);
#1153=FACE_OUTER_BOUND('',#1712,.T.);
#1154=FACE_OUTER_BOUND('',#1713,.T.);
#1155=FACE_OUTER_BOUND('',#1714,.T.);
#1156=FACE_OUTER_BOUND('',#1715,.T.);
#1157=FACE_OUTER_BOUND('',#1716,.T.);
#1158=FACE_OUTER_BOUND('',#1717,.T.);
#1159=FACE_OUTER_BOUND('',#1718,.T.);
#1160=FACE_OUTER_BOUND('',#1719,.T.);
#1161=FACE_OUTER_BOUND('',#1720,.T.);
#1162=FACE_OUTER_BOUND('',#1721,.T.);
#1163=FACE_OUTER_BOUND('',#1723,.T.);
#1164=FACE_OUTER_BOUND('',#1724,.T.);
#1165=FACE_OUTER_BOUND('',#1727,.T.);
#1166=FACE_OUTER_BOUND('',#1728,.T.);
#1167=FACE_OUTER_BOUND('',#1729,.T.);
#1168=FACE_OUTER_BOUND('',#1730,.T.);
#1169=FACE_OUTER_BOUND('',#1732,.T.);
#1170=FACE_OUTER_BOUND('',#1733,.T.);
#1171=FACE_OUTER_BOUND('',#1734,.T.);
#1172=FACE_OUTER_BOUND('',#1735,.T.);
#1173=FACE_OUTER_BOUND('',#1736,.T.);
#1174=FACE_OUTER_BOUND('',#1737,.T.);
#1175=FACE_OUTER_BOUND('',#1738,.T.);
#1176=FACE_OUTER_BOUND('',#1739,.T.);
#1177=FACE_OUTER_BOUND('',#1740,.T.);
#1178=FACE_OUTER_BOUND('',#1741,.T.);
#1179=FACE_OUTER_BOUND('',#1742,.T.);
#1180=FACE_OUTER_BOUND('',#1743,.T.);
#1181=FACE_OUTER_BOUND('',#1745,.T.);
#1182=FACE_OUTER_BOUND('',#1746,.T.);
#1183=FACE_OUTER_BOUND('',#1747,.T.);
#1184=FACE_OUTER_BOUND('',#1749,.T.);
#1185=FACE_OUTER_BOUND('',#1750,.T.);
#1186=FACE_OUTER_BOUND('',#1752,.T.);
#1187=FACE_OUTER_BOUND('',#1753,.T.);
#1188=FACE_OUTER_BOUND('',#1756,.T.);
#1189=FACE_OUTER_BOUND('',#1758,.T.);
#1190=FACE_OUTER_BOUND('',#1759,.T.);
#1191=FACE_OUTER_BOUND('',#1761,.T.);
#1192=FACE_OUTER_BOUND('',#1763,.T.);
#1193=FACE_OUTER_BOUND('',#1764,.T.);
#1194=FACE_OUTER_BOUND('',#1765,.T.);
#1195=FACE_OUTER_BOUND('',#1766,.T.);
#1196=FACE_OUTER_BOUND('',#1767,.T.);
#1197=FACE_OUTER_BOUND('',#1769,.T.);
#1198=FACE_OUTER_BOUND('',#1770,.T.);
#1199=FACE_OUTER_BOUND('',#1771,.T.);
#1200=FACE_OUTER_BOUND('',#1773,.T.);
#1201=FACE_OUTER_BOUND('',#1774,.T.);
#1202=FACE_OUTER_BOUND('',#1775,.T.);
#1203=FACE_OUTER_BOUND('',#1776,.T.);
#1204=FACE_OUTER_BOUND('',#1777,.T.);
#1205=FACE_OUTER_BOUND('',#1778,.T.);
#1206=FACE_OUTER_BOUND('',#1779,.T.);
#1207=FACE_OUTER_BOUND('',#1780,.T.);
#1208=FACE_OUTER_BOUND('',#1781,.T.);
#1209=FACE_OUTER_BOUND('',#1782,.T.);
#1210=FACE_OUTER_BOUND('',#1783,.T.);
#1211=FACE_OUTER_BOUND('',#1784,.T.);
#1212=FACE_OUTER_BOUND('',#1785,.T.);
#1213=FACE_OUTER_BOUND('',#1787,.T.);
#1214=FACE_OUTER_BOUND('',#1789,.T.);
#1215=FACE_OUTER_BOUND('',#1790,.T.);
#1216=FACE_OUTER_BOUND('',#1791,.T.);
#1217=FACE_OUTER_BOUND('',#1792,.T.);
#1218=FACE_OUTER_BOUND('',#1793,.T.);
#1219=FACE_OUTER_BOUND('',#1794,.T.);
#1220=FACE_OUTER_BOUND('',#1795,.T.);
#1221=FACE_OUTER_BOUND('',#1796,.T.);
#1222=FACE_OUTER_BOUND('',#1797,.T.);
#1223=FACE_OUTER_BOUND('',#1798,.T.);
#1224=FACE_OUTER_BOUND('',#1799,.T.);
#1225=FACE_OUTER_BOUND('',#1800,.T.);
#1226=FACE_OUTER_BOUND('',#1801,.T.);
#1227=FACE_OUTER_BOUND('',#1802,.T.);
#1228=FACE_OUTER_BOUND('',#1803,.T.);
#1229=FACE_OUTER_BOUND('',#1804,.T.);
#1230=FACE_OUTER_BOUND('',#1805,.T.);
#1231=FACE_OUTER_BOUND('',#1806,.T.);
#1232=FACE_OUTER_BOUND('',#1807,.T.);
#1233=FACE_OUTER_BOUND('',#1808,.T.);
#1234=FACE_OUTER_BOUND('',#1809,.T.);
#1235=FACE_OUTER_BOUND('',#1810,.T.);
#1236=FACE_OUTER_BOUND('',#1811,.T.);
#1237=FACE_OUTER_BOUND('',#1812,.T.);
#1238=FACE_OUTER_BOUND('',#1813,.T.);
#1239=FACE_OUTER_BOUND('',#1814,.T.);
#1240=FACE_OUTER_BOUND('',#1816,.T.);
#1241=FACE_OUTER_BOUND('',#1818,.T.);
#1242=FACE_OUTER_BOUND('',#1819,.T.);
#1243=FACE_OUTER_BOUND('',#1821,.T.);
#1244=FACE_OUTER_BOUND('',#1822,.T.);
#1245=FACE_OUTER_BOUND('',#1823,.T.);
#1246=FACE_OUTER_BOUND('',#1824,.T.);
#1247=FACE_OUTER_BOUND('',#1825,.T.);
#1248=FACE_OUTER_BOUND('',#1826,.T.);
#1249=FACE_OUTER_BOUND('',#1827,.T.);
#1250=FACE_OUTER_BOUND('',#1828,.T.);
#1251=FACE_OUTER_BOUND('',#1829,.T.);
#1252=FACE_OUTER_BOUND('',#1830,.T.);
#1253=FACE_OUTER_BOUND('',#1831,.T.);
#1254=FACE_OUTER_BOUND('',#1832,.T.);
#1255=FACE_OUTER_BOUND('',#1833,.T.);
#1256=FACE_OUTER_BOUND('',#1834,.T.);
#1257=FACE_OUTER_BOUND('',#1835,.T.);
#1258=FACE_OUTER_BOUND('',#1836,.T.);
#1259=FACE_OUTER_BOUND('',#1837,.T.);
#1260=FACE_OUTER_BOUND('',#1838,.T.);
#1261=FACE_OUTER_BOUND('',#1839,.T.);
#1262=FACE_OUTER_BOUND('',#1840,.T.);
#1263=FACE_OUTER_BOUND('',#1841,.T.);
#1264=FACE_OUTER_BOUND('',#1842,.T.);
#1265=FACE_OUTER_BOUND('',#1843,.T.);
#1266=FACE_OUTER_BOUND('',#1844,.T.);
#1267=FACE_OUTER_BOUND('',#1845,.T.);
#1268=FACE_OUTER_BOUND('',#1846,.T.);
#1269=FACE_OUTER_BOUND('',#1847,.T.);
#1270=FACE_OUTER_BOUND('',#1848,.T.);
#1271=FACE_OUTER_BOUND('',#1858,.T.);
#1272=FACE_OUTER_BOUND('',#1860,.T.);
#1273=FACE_OUTER_BOUND('',#1862,.T.);
#1274=FACE_OUTER_BOUND('',#1864,.T.);
#1275=FACE_OUTER_BOUND('',#1866,.T.);
#1276=FACE_OUTER_BOUND('',#1869,.T.);
#1277=FACE_OUTER_BOUND('',#1870,.T.);
#1278=FACE_OUTER_BOUND('',#1871,.T.);
#1279=FACE_OUTER_BOUND('',#1872,.T.);
#1280=FACE_OUTER_BOUND('',#1873,.T.);
#1281=FACE_OUTER_BOUND('',#1874,.T.);
#1282=FACE_OUTER_BOUND('',#1875,.T.);
#1283=FACE_OUTER_BOUND('',#1876,.T.);
#1284=FACE_OUTER_BOUND('',#1877,.T.);
#1285=FACE_OUTER_BOUND('',#1878,.T.);
#1286=FACE_OUTER_BOUND('',#1879,.T.);
#1287=FACE_OUTER_BOUND('',#1880,.T.);
#1288=FACE_OUTER_BOUND('',#1881,.T.);
#1289=FACE_OUTER_BOUND('',#1882,.T.);
#1290=FACE_OUTER_BOUND('',#1883,.T.);
#1291=FACE_OUTER_BOUND('',#1884,.T.);
#1292=FACE_OUTER_BOUND('',#1885,.T.);
#1293=FACE_OUTER_BOUND('',#1886,.T.);
#1294=FACE_OUTER_BOUND('',#1887,.T.);
#1295=FACE_OUTER_BOUND('',#1888,.T.);
#1296=FACE_OUTER_BOUND('',#1889,.T.);
#1297=FACE_OUTER_BOUND('',#1890,.T.);
#1298=FACE_OUTER_BOUND('',#1891,.T.);
#1299=FACE_OUTER_BOUND('',#1892,.T.);
#1300=FACE_OUTER_BOUND('',#1893,.T.);
#1301=FACE_OUTER_BOUND('',#1894,.T.);
#1302=FACE_OUTER_BOUND('',#1895,.T.);
#1303=FACE_OUTER_BOUND('',#1896,.T.);
#1304=FACE_OUTER_BOUND('',#1897,.T.);
#1305=FACE_OUTER_BOUND('',#1898,.T.);
#1306=FACE_OUTER_BOUND('',#1899,.T.);
#1307=FACE_OUTER_BOUND('',#1900,.T.);
#1308=FACE_OUTER_BOUND('',#1901,.T.);
#1309=FACE_OUTER_BOUND('',#1902,.T.);
#1310=FACE_OUTER_BOUND('',#1903,.T.);
#1311=FACE_OUTER_BOUND('',#1904,.T.);
#1312=FACE_OUTER_BOUND('',#1905,.T.);
#1313=FACE_OUTER_BOUND('',#1906,.T.);
#1314=FACE_OUTER_BOUND('',#1907,.T.);
#1315=FACE_OUTER_BOUND('',#1908,.T.);
#1316=FACE_OUTER_BOUND('',#1909,.T.);
#1317=FACE_OUTER_BOUND('',#1910,.T.);
#1318=FACE_OUTER_BOUND('',#1911,.T.);
#1319=FACE_OUTER_BOUND('',#1913,.T.);
#1320=FACE_OUTER_BOUND('',#1915,.T.);
#1321=FACE_OUTER_BOUND('',#1917,.T.);
#1322=FACE_OUTER_BOUND('',#1918,.T.);
#1323=FACE_OUTER_BOUND('',#1919,.T.);
#1324=FACE_OUTER_BOUND('',#1920,.T.);
#1325=FACE_OUTER_BOUND('',#1921,.T.);
#1326=FACE_OUTER_BOUND('',#1922,.T.);
#1327=FACE_OUTER_BOUND('',#1924,.T.);
#1328=FACE_OUTER_BOUND('',#1925,.T.);
#1329=FACE_OUTER_BOUND('',#1927,.T.);
#1330=FACE_OUTER_BOUND('',#1928,.T.);
#1331=FACE_OUTER_BOUND('',#1929,.T.);
#1332=FACE_OUTER_BOUND('',#1930,.T.);
#1333=FACE_OUTER_BOUND('',#1931,.T.);
#1334=FACE_OUTER_BOUND('',#1932,.T.);
#1335=FACE_OUTER_BOUND('',#1933,.T.);
#1336=FACE_OUTER_BOUND('',#1934,.T.);
#1337=FACE_OUTER_BOUND('',#1935,.T.);
#1338=FACE_OUTER_BOUND('',#1936,.T.);
#1339=FACE_OUTER_BOUND('',#1937,.T.);
#1340=FACE_OUTER_BOUND('',#1938,.T.);
#1341=FACE_OUTER_BOUND('',#1940,.T.);
#1342=FACE_OUTER_BOUND('',#1941,.T.);
#1343=FACE_OUTER_BOUND('',#1942,.T.);
#1344=FACE_OUTER_BOUND('',#1943,.T.);
#1345=FACE_OUTER_BOUND('',#1944,.T.);
#1346=FACE_OUTER_BOUND('',#1945,.T.);
#1347=FACE_OUTER_BOUND('',#1946,.T.);
#1348=FACE_OUTER_BOUND('',#1948,.T.);
#1349=FACE_OUTER_BOUND('',#1950,.T.);
#1350=FACE_OUTER_BOUND('',#1951,.T.);
#1351=FACE_OUTER_BOUND('',#1953,.T.);
#1352=FACE_OUTER_BOUND('',#1954,.T.);
#1353=FACE_OUTER_BOUND('',#1955,.T.);
#1354=FACE_OUTER_BOUND('',#1956,.T.);
#1355=FACE_OUTER_BOUND('',#1957,.T.);
#1356=FACE_OUTER_BOUND('',#1958,.T.);
#1357=FACE_OUTER_BOUND('',#1959,.T.);
#1358=FACE_OUTER_BOUND('',#1960,.T.);
#1359=FACE_OUTER_BOUND('',#1962,.T.);
#1360=FACE_OUTER_BOUND('',#1963,.T.);
#1361=FACE_OUTER_BOUND('',#1964,.T.);
#1362=FACE_OUTER_BOUND('',#1965,.T.);
#1363=FACE_OUTER_BOUND('',#1966,.T.);
#1364=FACE_OUTER_BOUND('',#1968,.T.);
#1365=FACE_OUTER_BOUND('',#1969,.T.);
#1366=FACE_OUTER_BOUND('',#1970,.T.);
#1367=FACE_OUTER_BOUND('',#1971,.T.);
#1368=FACE_OUTER_BOUND('',#1972,.T.);
#1369=FACE_OUTER_BOUND('',#1973,.T.);
#1370=FACE_OUTER_BOUND('',#1974,.T.);
#1371=FACE_OUTER_BOUND('',#1975,.T.);
#1372=FACE_OUTER_BOUND('',#1976,.T.);
#1373=FACE_OUTER_BOUND('',#1977,.T.);
#1374=FACE_OUTER_BOUND('',#1978,.T.);
#1375=FACE_OUTER_BOUND('',#1979,.T.);
#1376=FACE_OUTER_BOUND('',#1980,.T.);
#1377=FACE_OUTER_BOUND('',#1981,.T.);
#1378=FACE_OUTER_BOUND('',#1982,.T.);
#1379=FACE_OUTER_BOUND('',#1983,.T.);
#1380=FACE_OUTER_BOUND('',#1984,.T.);
#1381=FACE_OUTER_BOUND('',#1985,.T.);
#1382=FACE_OUTER_BOUND('',#1986,.T.);
#1383=FACE_OUTER_BOUND('',#1987,.T.);
#1384=FACE_OUTER_BOUND('',#1988,.T.);
#1385=FACE_OUTER_BOUND('',#1989,.T.);
#1386=FACE_OUTER_BOUND('',#1990,.T.);
#1387=FACE_OUTER_BOUND('',#1991,.T.);
#1388=FACE_OUTER_BOUND('',#1992,.T.);
#1389=FACE_OUTER_BOUND('',#1993,.T.);
#1390=FACE_OUTER_BOUND('',#1994,.T.);
#1391=FACE_OUTER_BOUND('',#1995,.T.);
#1392=FACE_OUTER_BOUND('',#1996,.T.);
#1393=FACE_OUTER_BOUND('',#1997,.T.);
#1394=FACE_OUTER_BOUND('',#1998,.T.);
#1395=FACE_OUTER_BOUND('',#1999,.T.);
#1396=FACE_OUTER_BOUND('',#2000,.T.);
#1397=FACE_OUTER_BOUND('',#2002,.T.);
#1398=FACE_OUTER_BOUND('',#2004,.T.);
#1399=FACE_OUTER_BOUND('',#2005,.T.);
#1400=FACE_OUTER_BOUND('',#2006,.T.);
#1401=FACE_OUTER_BOUND('',#2007,.T.);
#1402=FACE_OUTER_BOUND('',#2009,.T.);
#1403=FACE_OUTER_BOUND('',#2010,.T.);
#1404=FACE_OUTER_BOUND('',#2011,.T.);
#1405=FACE_OUTER_BOUND('',#2013,.T.);
#1406=FACE_OUTER_BOUND('',#2014,.T.);
#1407=FACE_OUTER_BOUND('',#2016,.T.);
#1408=FACE_OUTER_BOUND('',#2017,.T.);
#1409=FACE_OUTER_BOUND('',#2018,.T.);
#1410=FACE_OUTER_BOUND('',#2019,.T.);
#1411=FACE_OUTER_BOUND('',#2020,.T.);
#1412=FACE_OUTER_BOUND('',#2021,.T.);
#1413=FACE_OUTER_BOUND('',#2022,.T.);
#1414=FACE_OUTER_BOUND('',#2023,.T.);
#1415=FACE_OUTER_BOUND('',#2024,.T.);
#1416=FACE_OUTER_BOUND('',#2025,.T.);
#1417=FACE_OUTER_BOUND('',#2026,.T.);
#1418=FACE_OUTER_BOUND('',#2027,.T.);
#1419=FACE_OUTER_BOUND('',#2029,.T.);
#1420=FACE_OUTER_BOUND('',#2030,.T.);
#1421=FACE_OUTER_BOUND('',#2031,.T.);
#1422=FACE_OUTER_BOUND('',#2032,.T.);
#1423=FACE_OUTER_BOUND('',#2034,.T.);
#1424=FACE_OUTER_BOUND('',#2035,.T.);
#1425=FACE_OUTER_BOUND('',#2041,.T.);
#1426=FACE_OUTER_BOUND('',#2043,.T.);
#1427=FACE_OUTER_BOUND('',#2044,.T.);
#1428=FACE_OUTER_BOUND('',#2045,.T.);
#1429=FACE_OUTER_BOUND('',#2047,.T.);
#1430=FACE_OUTER_BOUND('',#2053,.T.);
#1431=FACE_OUTER_BOUND('',#2054,.T.);
#1432=FACE_OUTER_BOUND('',#2055,.T.);
#1433=FACE_OUTER_BOUND('',#2056,.T.);
#1434=FACE_OUTER_BOUND('',#2057,.T.);
#1435=FACE_OUTER_BOUND('',#2058,.T.);
#1436=FACE_OUTER_BOUND('',#2059,.T.);
#1437=FACE_OUTER_BOUND('',#2060,.T.);
#1438=FACE_OUTER_BOUND('',#2062,.T.);
#1439=FACE_OUTER_BOUND('',#2063,.T.);
#1440=FACE_OUTER_BOUND('',#2065,.T.);
#1441=FACE_OUTER_BOUND('',#2066,.T.);
#1442=FACE_OUTER_BOUND('',#2067,.T.);
#1443=FACE_OUTER_BOUND('',#2068,.T.);
#1444=FACE_OUTER_BOUND('',#2069,.T.);
#1445=FACE_OUTER_BOUND('',#2070,.T.);
#1446=FACE_OUTER_BOUND('',#2071,.T.);
#1447=FACE_OUTER_BOUND('',#2072,.T.);
#1448=FACE_OUTER_BOUND('',#2073,.T.);
#1449=FACE_OUTER_BOUND('',#2074,.T.);
#1450=FACE_OUTER_BOUND('',#2075,.T.);
#1451=FACE_OUTER_BOUND('',#2076,.T.);
#1452=FACE_OUTER_BOUND('',#2077,.T.);
#1453=FACE_OUTER_BOUND('',#2078,.T.);
#1454=FACE_OUTER_BOUND('',#2079,.T.);
#1455=FACE_OUTER_BOUND('',#2080,.T.);
#1456=FACE_OUTER_BOUND('',#2081,.T.);
#1457=FACE_OUTER_BOUND('',#2082,.T.);
#1458=FACE_OUTER_BOUND('',#2083,.T.);
#1459=FACE_OUTER_BOUND('',#2084,.T.);
#1460=FACE_OUTER_BOUND('',#2085,.T.);
#1461=FACE_OUTER_BOUND('',#2086,.T.);
#1462=FACE_OUTER_BOUND('',#2087,.T.);
#1463=FACE_OUTER_BOUND('',#2088,.T.);
#1464=FACE_OUTER_BOUND('',#2089,.T.);
#1465=FACE_OUTER_BOUND('',#2090,.T.);
#1466=FACE_OUTER_BOUND('',#2091,.T.);
#1467=FACE_OUTER_BOUND('',#2092,.T.);
#1468=FACE_OUTER_BOUND('',#2093,.T.);
#1469=FACE_OUTER_BOUND('',#2094,.T.);
#1470=FACE_OUTER_BOUND('',#2095,.T.);
#1471=FACE_OUTER_BOUND('',#2096,.T.);
#1472=FACE_OUTER_BOUND('',#2097,.T.);
#1473=FACE_OUTER_BOUND('',#2098,.T.);
#1474=FACE_OUTER_BOUND('',#2099,.T.);
#1475=FACE_OUTER_BOUND('',#2100,.T.);
#1476=FACE_OUTER_BOUND('',#2101,.T.);
#1477=FACE_OUTER_BOUND('',#2102,.T.);
#1478=FACE_OUTER_BOUND('',#2103,.T.);
#1479=FACE_OUTER_BOUND('',#2104,.T.);
#1480=FACE_OUTER_BOUND('',#2105,.T.);
#1481=FACE_OUTER_BOUND('',#2106,.T.);
#1482=FACE_OUTER_BOUND('',#2107,.T.);
#1483=FACE_OUTER_BOUND('',#2108,.T.);
#1484=FACE_OUTER_BOUND('',#2109,.T.);
#1485=FACE_OUTER_BOUND('',#2110,.T.);
#1486=FACE_OUTER_BOUND('',#2111,.T.);
#1487=FACE_OUTER_BOUND('',#2112,.T.);
#1488=FACE_OUTER_BOUND('',#2113,.T.);
#1489=FACE_OUTER_BOUND('',#2114,.T.);
#1490=FACE_OUTER_BOUND('',#2115,.T.);
#1491=FACE_OUTER_BOUND('',#2117,.T.);
#1492=FACE_OUTER_BOUND('',#2119,.T.);
#1493=FACE_OUTER_BOUND('',#2120,.T.);
#1494=FACE_OUTER_BOUND('',#2121,.T.);
#1495=FACE_OUTER_BOUND('',#2122,.T.);
#1496=FACE_OUTER_BOUND('',#2123,.T.);
#1497=FACE_OUTER_BOUND('',#2124,.T.);
#1498=FACE_OUTER_BOUND('',#2125,.T.);
#1499=FACE_OUTER_BOUND('',#2126,.T.);
#1500=FACE_OUTER_BOUND('',#2127,.T.);
#1501=FACE_OUTER_BOUND('',#2129,.T.);
#1502=FACE_OUTER_BOUND('',#2130,.T.);
#1503=FACE_OUTER_BOUND('',#2131,.T.);
#1504=FACE_OUTER_BOUND('',#2132,.T.);
#1505=FACE_OUTER_BOUND('',#2133,.T.);
#1506=FACE_OUTER_BOUND('',#2134,.T.);
#1507=FACE_OUTER_BOUND('',#2135,.T.);
#1508=FACE_OUTER_BOUND('',#2136,.T.);
#1509=FACE_OUTER_BOUND('',#2137,.T.);
#1510=FACE_OUTER_BOUND('',#2138,.T.);
#1511=FACE_OUTER_BOUND('',#2139,.T.);
#1512=FACE_OUTER_BOUND('',#2140,.T.);
#1513=FACE_OUTER_BOUND('',#2141,.T.);
#1514=FACE_OUTER_BOUND('',#2142,.T.);
#1515=FACE_OUTER_BOUND('',#2143,.T.);
#1516=FACE_OUTER_BOUND('',#2144,.T.);
#1517=FACE_OUTER_BOUND('',#2145,.T.);
#1518=FACE_OUTER_BOUND('',#2146,.T.);
#1519=FACE_OUTER_BOUND('',#2147,.T.);
#1520=FACE_OUTER_BOUND('',#2148,.T.);
#1521=FACE_OUTER_BOUND('',#2149,.T.);
#1522=FACE_OUTER_BOUND('',#2150,.T.);
#1523=FACE_OUTER_BOUND('',#2151,.T.);
#1524=FACE_OUTER_BOUND('',#2152,.T.);
#1525=FACE_OUTER_BOUND('',#2153,.T.);
#1526=FACE_OUTER_BOUND('',#2154,.T.);
#1527=FACE_OUTER_BOUND('',#2155,.T.);
#1528=FACE_OUTER_BOUND('',#2156,.T.);
#1529=FACE_OUTER_BOUND('',#2158,.T.);
#1530=FACE_OUTER_BOUND('',#2159,.T.);
#1531=FACE_OUTER_BOUND('',#2160,.T.);
#1532=FACE_OUTER_BOUND('',#2161,.T.);
#1533=FACE_OUTER_BOUND('',#2163,.T.);
#1534=FACE_OUTER_BOUND('',#2164,.T.);
#1535=FACE_OUTER_BOUND('',#2166,.T.);
#1536=FACE_OUTER_BOUND('',#2167,.T.);
#1537=FACE_OUTER_BOUND('',#2168,.T.);
#1538=FACE_OUTER_BOUND('',#2169,.T.);
#1539=FACE_OUTER_BOUND('',#2170,.T.);
#1540=FACE_OUTER_BOUND('',#2171,.T.);
#1541=FACE_OUTER_BOUND('',#2173,.T.);
#1542=FACE_OUTER_BOUND('',#2174,.T.);
#1543=FACE_OUTER_BOUND('',#2175,.T.);
#1544=FACE_OUTER_BOUND('',#2176,.T.);
#1545=FACE_OUTER_BOUND('',#2177,.T.);
#1546=FACE_OUTER_BOUND('',#2178,.T.);
#1547=FACE_OUTER_BOUND('',#2180,.T.);
#1548=FACE_OUTER_BOUND('',#2181,.T.);
#1549=FACE_OUTER_BOUND('',#2182,.T.);
#1550=FACE_OUTER_BOUND('',#2183,.T.);
#1551=FACE_OUTER_BOUND('',#2184,.T.);
#1552=FACE_OUTER_BOUND('',#2185,.T.);
#1553=FACE_OUTER_BOUND('',#2186,.T.);
#1554=FACE_OUTER_BOUND('',#2188,.T.);
#1555=FACE_OUTER_BOUND('',#2189,.T.);
#1556=FACE_OUTER_BOUND('',#2191,.T.);
#1557=FACE_OUTER_BOUND('',#2193,.T.);
#1558=FACE_OUTER_BOUND('',#2194,.T.);
#1559=FACE_OUTER_BOUND('',#2195,.T.);
#1560=FACE_OUTER_BOUND('',#2196,.T.);
#1561=FACE_OUTER_BOUND('',#2197,.T.);
#1562=FACE_OUTER_BOUND('',#2198,.T.);
#1563=FACE_OUTER_BOUND('',#2199,.T.);
#1564=FACE_OUTER_BOUND('',#2200,.T.);
#1565=FACE_OUTER_BOUND('',#2201,.T.);
#1566=FACE_OUTER_BOUND('',#2202,.T.);
#1567=FACE_OUTER_BOUND('',#2203,.T.);
#1568=FACE_OUTER_BOUND('',#2204,.T.);
#1569=FACE_OUTER_BOUND('',#2205,.T.);
#1570=FACE_OUTER_BOUND('',#2206,.T.);
#1571=FACE_OUTER_BOUND('',#2207,.T.);
#1572=FACE_OUTER_BOUND('',#2208,.T.);
#1573=FACE_OUTER_BOUND('',#2209,.T.);
#1574=FACE_OUTER_BOUND('',#2210,.T.);
#1575=FACE_OUTER_BOUND('',#2211,.T.);
#1576=EDGE_LOOP('',(#6424,#6425,#6426,#6427));
#1577=EDGE_LOOP('',(#6428,#6429,#6430,#6431));
#1578=EDGE_LOOP('',(#6432,#6433,#6434,#6435));
#1579=EDGE_LOOP('',(#6436,#6437,#6438,#6439));
#1580=EDGE_LOOP('',(#6440,#6441,#6442,#6443));
#1581=EDGE_LOOP('',(#6444,#6445,#6446,#6447));
#1582=EDGE_LOOP('',(#6448,#6449,#6450,#6451));
#1583=EDGE_LOOP('',(#6452,#6453,#6454,#6455));
#1584=EDGE_LOOP('',(#6456,#6457,#6458,#6459));
#1585=EDGE_LOOP('',(#6460,#6461,#6462,#6463));
#1586=EDGE_LOOP('',(#6464,#6465,#6466,#6467));
#1587=EDGE_LOOP('',(#6468,#6469,#6470,#6471));
#1588=EDGE_LOOP('',(#6472,#6473,#6474,#6475));
#1589=EDGE_LOOP('',(#6476,#6477,#6478,#6479));
#1590=EDGE_LOOP('',(#6480,#6481,#6482,#6483));
#1591=EDGE_LOOP('',(#6484,#6485,#6486,#6487));
#1592=EDGE_LOOP('',(#6488,#6489,#6490,#6491));
#1593=EDGE_LOOP('',(#6492,#6493,#6494,#6495));
#1594=EDGE_LOOP('',(#6496,#6497,#6498,#6499));
#1595=EDGE_LOOP('',(#6500,#6501,#6502,#6503));
#1596=EDGE_LOOP('',(#6504,#6505,#6506,#6507));
#1597=EDGE_LOOP('',(#6508,#6509,#6510,#6511));
#1598=EDGE_LOOP('',(#6512,#6513,#6514,#6515));
#1599=EDGE_LOOP('',(#6516,#6517,#6518,#6519));
#1600=EDGE_LOOP('',(#6520,#6521,#6522,#6523));
#1601=EDGE_LOOP('',(#6524,#6525,#6526,#6527));
#1602=EDGE_LOOP('',(#6528,#6529,#6530,#6531));
#1603=EDGE_LOOP('',(#6532,#6533,#6534,#6535));
#1604=EDGE_LOOP('',(#6536,#6537,#6538,#6539));
#1605=EDGE_LOOP('',(#6540,#6541,#6542,#6543));
#1606=EDGE_LOOP('',(#6544,#6545,#6546,#6547));
#1607=EDGE_LOOP('',(#6548,#6549,#6550,#6551));
#1608=EDGE_LOOP('',(#6552,#6553,#6554,#6555));
#1609=EDGE_LOOP('',(#6556,#6557,#6558,#6559));
#1610=EDGE_LOOP('',(#6560,#6561,#6562,#6563));
#1611=EDGE_LOOP('',(#6564,#6565,#6566,#6567));
#1612=EDGE_LOOP('',(#6568,#6569,#6570,#6571));
#1613=EDGE_LOOP('',(#6572,#6573,#6574,#6575));
#1614=EDGE_LOOP('',(#6576,#6577,#6578,#6579));
#1615=EDGE_LOOP('',(#6580,#6581,#6582,#6583));
#1616=EDGE_LOOP('',(#6584,#6585,#6586,#6587));
#1617=EDGE_LOOP('',(#6588,#6589,#6590,#6591));
#1618=EDGE_LOOP('',(#6592,#6593,#6594,#6595));
#1619=EDGE_LOOP('',(#6596,#6597,#6598,#6599));
#1620=EDGE_LOOP('',(#6600,#6601,#6602,#6603));
#1621=EDGE_LOOP('',(#6604,#6605,#6606,#6607));
#1622=EDGE_LOOP('',(#6608,#6609,#6610,#6611));
#1623=EDGE_LOOP('',(#6612,#6613,#6614,#6615));
#1624=EDGE_LOOP('',(#6616,#6617,#6618,#6619));
#1625=EDGE_LOOP('',(#6620,#6621,#6622,#6623));
#1626=EDGE_LOOP('',(#6624,#6625,#6626,#6627));
#1627=EDGE_LOOP('',(#6628,#6629,#6630,#6631));
#1628=EDGE_LOOP('',(#6632,#6633,#6634,#6635));
#1629=EDGE_LOOP('',(#6636,#6637,#6638,#6639));
#1630=EDGE_LOOP('',(#6640,#6641,#6642,#6643));
#1631=EDGE_LOOP('',(#6644,#6645,#6646,#6647));
#1632=EDGE_LOOP('',(#6648,#6649,#6650,#6651));
#1633=EDGE_LOOP('',(#6652,#6653,#6654,#6655));
#1634=EDGE_LOOP('',(#6656,#6657,#6658,#6659));
#1635=EDGE_LOOP('',(#6660,#6661,#6662,#6663));
#1636=EDGE_LOOP('',(#6664,#6665,#6666,#6667));
#1637=EDGE_LOOP('',(#6668,#6669,#6670,#6671));
#1638=EDGE_LOOP('',(#6672,#6673,#6674,#6675));
#1639=EDGE_LOOP('',(#6676,#6677,#6678,#6679));
#1640=EDGE_LOOP('',(#6680,#6681,#6682,#6683));
#1641=EDGE_LOOP('',(#6684,#6685,#6686,#6687));
#1642=EDGE_LOOP('',(#6688,#6689,#6690,#6691));
#1643=EDGE_LOOP('',(#6692,#6693,#6694,#6695));
#1644=EDGE_LOOP('',(#6696,#6697,#6698,#6699));
#1645=EDGE_LOOP('',(#6700,#6701,#6702,#6703));
#1646=EDGE_LOOP('',(#6704,#6705,#6706,#6707));
#1647=EDGE_LOOP('',(#6708,#6709,#6710,#6711));
#1648=EDGE_LOOP('',(#6712,#6713,#6714,#6715));
#1649=EDGE_LOOP('',(#6716,#6717,#6718,#6719));
#1650=EDGE_LOOP('',(#6720,#6721,#6722,#6723));
#1651=EDGE_LOOP('',(#6724,#6725,#6726,#6727));
#1652=EDGE_LOOP('',(#6728,#6729,#6730,#6731));
#1653=EDGE_LOOP('',(#6732,#6733,#6734,#6735));
#1654=EDGE_LOOP('',(#6736,#6737,#6738,#6739));
#1655=EDGE_LOOP('',(#6740,#6741,#6742,#6743));
#1656=EDGE_LOOP('',(#6744,#6745,#6746,#6747));
#1657=EDGE_LOOP('',(#6748,#6749,#6750,#6751));
#1658=EDGE_LOOP('',(#6752,#6753,#6754,#6755));
#1659=EDGE_LOOP('',(#6756,#6757,#6758,#6759));
#1660=EDGE_LOOP('',(#6760,#6761,#6762,#6763));
#1661=EDGE_LOOP('',(#6764,#6765,#6766,#6767));
#1662=EDGE_LOOP('',(#6768,#6769,#6770,#6771));
#1663=EDGE_LOOP('',(#6772,#6773,#6774,#6775));
#1664=EDGE_LOOP('',(#6776,#6777,#6778,#6779));
#1665=EDGE_LOOP('',(#6780,#6781,#6782,#6783));
#1666=EDGE_LOOP('',(#6784,#6785,#6786,#6787));
#1667=EDGE_LOOP('',(#6788,#6789,#6790,#6791));
#1668=EDGE_LOOP('',(#6792,#6793,#6794,#6795));
#1669=EDGE_LOOP('',(#6796,#6797,#6798,#6799));
#1670=EDGE_LOOP('',(#6800,#6801,#6802,#6803));
#1671=EDGE_LOOP('',(#6804,#6805,#6806,#6807));
#1672=EDGE_LOOP('',(#6808,#6809,#6810,#6811));
#1673=EDGE_LOOP('',(#6812,#6813,#6814,#6815));
#1674=EDGE_LOOP('',(#6816,#6817,#6818,#6819));
#1675=EDGE_LOOP('',(#6820,#6821,#6822,#6823));
#1676=EDGE_LOOP('',(#6824,#6825,#6826,#6827));
#1677=EDGE_LOOP('',(#6828,#6829,#6830,#6831));
#1678=EDGE_LOOP('',(#6832,#6833,#6834,#6835));
#1679=EDGE_LOOP('',(#6836,#6837,#6838,#6839));
#1680=EDGE_LOOP('',(#6840,#6841,#6842,#6843));
#1681=EDGE_LOOP('',(#6844,#6845,#6846,#6847));
#1682=EDGE_LOOP('',(#6848,#6849,#6850,#6851));
#1683=EDGE_LOOP('',(#6852,#6853,#6854,#6855));
#1684=EDGE_LOOP('',(#6856,#6857,#6858,#6859));
#1685=EDGE_LOOP('',(#6860,#6861,#6862,#6863));
#1686=EDGE_LOOP('',(#6864,#6865,#6866,#6867));
#1687=EDGE_LOOP('',(#6868,#6869,#6870,#6871));
#1688=EDGE_LOOP('',(#6872,#6873,#6874,#6875));
#1689=EDGE_LOOP('',(#6876,#6877,#6878,#6879));
#1690=EDGE_LOOP('',(#6880,#6881,#6882,#6883));
#1691=EDGE_LOOP('',(#6884,#6885,#6886,#6887));
#1692=EDGE_LOOP('',(#6888,#6889,#6890,#6891));
#1693=EDGE_LOOP('',(#6892,#6893,#6894,#6895));
#1694=EDGE_LOOP('',(#6896,#6897,#6898,#6899));
#1695=EDGE_LOOP('',(#6900,#6901,#6902,#6903));
#1696=EDGE_LOOP('',(#6904,#6905,#6906,#6907));
#1697=EDGE_LOOP('',(#6908,#6909,#6910,#6911,#6912));
#1698=EDGE_LOOP('',(#6913,#6914,#6915,#6916,#6917,#6918,#6919,#6920,#6921,
#6922,#6923,#6924,#6925,#6926,#6927,#6928,#6929,#6930,#6931,#6932,#6933,
#6934,#6935,#6936,#6937,#6938,#6939,#6940,#6941,#6942,#6943,#6944,#6945,
#6946,#6947,#6948,#6949,#6950,#6951,#6952,#6953,#6954,#6955,#6956,#6957,
#6958,#6959,#6960,#6961,#6962,#6963,#6964,#6965,#6966,#6967,#6968,#6969,
#6970,#6971,#6972,#6973,#6974,#6975,#6976,#6977,#6978,#6979,#6980,#6981,
#6982,#6983,#6984,#6985,#6986,#6987,#6988,#6989,#6990,#6991,#6992,#6993,
#6994,#6995,#6996,#6997,#6998,#6999,#7000,#7001,#7002,#7003,#7004,#7005,
#7006,#7007,#7008,#7009,#7010,#7011,#7012,#7013,#7014,#7015,#7016,#7017,
#7018,#7019,#7020,#7021,#7022,#7023,#7024,#7025,#7026,#7027,#7028,#7029,
#7030,#7031,#7032));
#1699=EDGE_LOOP('',(#7033,#7034,#7035,#7036,#7037));
#1700=EDGE_LOOP('',(#7038));
#1701=EDGE_LOOP('',(#7039,#7040,#7041,#7042,#7043,#7044,#7045,#7046,#7047,
#7048));
#1702=EDGE_LOOP('',(#7049,#7050,#7051));
#1703=EDGE_LOOP('',(#7052,#7053,#7054,#7055,#7056,#7057));
#1704=EDGE_LOOP('',(#7058,#7059,#7060));
#1705=EDGE_LOOP('',(#7061,#7062,#7063));
#1706=EDGE_LOOP('',(#7064,#7065,#7066,#7067,#7068,#7069,#7070));
#1707=EDGE_LOOP('',(#7071,#7072,#7073));
#1708=EDGE_LOOP('',(#7074,#7075,#7076,#7077));
#1709=EDGE_LOOP('',(#7078));
#1710=EDGE_LOOP('',(#7079,#7080,#7081,#7082,#7083,#7084,#7085,#7086,#7087,
#7088,#7089,#7090,#7091,#7092,#7093,#7094,#7095,#7096,#7097,#7098,#7099,
#7100,#7101,#7102,#7103,#7104,#7105,#7106,#7107,#7108,#7109,#7110,#7111,
#7112,#7113,#7114,#7115,#7116,#7117,#7118,#7119,#7120,#7121,#7122,#7123,
#7124,#7125,#7126,#7127,#7128,#7129,#7130,#7131,#7132,#7133,#7134,#7135,
#7136,#7137,#7138,#7139,#7140,#7141,#7142,#7143,#7144,#7145,#7146,#7147,
#7148,#7149,#7150,#7151,#7152,#7153,#7154,#7155,#7156,#7157,#7158,#7159,
#7160,#7161,#7162,#7163,#7164,#7165,#7166,#7167,#7168,#7169,#7170,#7171,
#7172,#7173,#7174,#7175,#7176,#7177,#7178,#7179,#7180,#7181,#7182,#7183,
#7184,#7185,#7186,#7187,#7188,#7189,#7190,#7191,#7192,#7193,#7194,#7195,
#7196,#7197,#7198));
#1711=EDGE_LOOP('',(#7199,#7200,#7201));
#1712=EDGE_LOOP('',(#7202,#7203,#7204,#7205));
#1713=EDGE_LOOP('',(#7206,#7207,#7208,#7209));
#1714=EDGE_LOOP('',(#7210,#7211,#7212,#7213));
#1715=EDGE_LOOP('',(#7214,#7215,#7216));
#1716=EDGE_LOOP('',(#7217,#7218,#7219));
#1717=EDGE_LOOP('',(#7220,#7221,#7222,#7223));
#1718=EDGE_LOOP('',(#7224,#7225,#7226,#7227));
#1719=EDGE_LOOP('',(#7228,#7229,#7230,#7231));
#1720=EDGE_LOOP('',(#7232,#7233,#7234));
#1721=EDGE_LOOP('',(#7235));
#1722=EDGE_LOOP('',(#7236));
#1723=EDGE_LOOP('',(#7237,#7238,#7239,#7240));
#1724=EDGE_LOOP('',(#7241,#7242,#7243,#7244));
#1725=EDGE_LOOP('',(#7245,#7246));
#1726=EDGE_LOOP('',(#7247,#7248));
#1727=EDGE_LOOP('',(#7249,#7250,#7251,#7252));
#1728=EDGE_LOOP('',(#7253,#7254,#7255,#7256));
#1729=EDGE_LOOP('',(#7257,#7258,#7259,#7260,#7261,#7262));
#1730=EDGE_LOOP('',(#7263));
#1731=EDGE_LOOP('',(#7264,#7265,#7266,#7267));
#1732=EDGE_LOOP('',(#7268,#7269,#7270,#7271));
#1733=EDGE_LOOP('',(#7272,#7273,#7274,#7275));
#1734=EDGE_LOOP('',(#7276,#7277,#7278,#7279));
#1735=EDGE_LOOP('',(#7280,#7281,#7282,#7283));
#1736=EDGE_LOOP('',(#7284,#7285,#7286,#7287));
#1737=EDGE_LOOP('',(#7288,#7289,#7290,#7291));
#1738=EDGE_LOOP('',(#7292,#7293,#7294,#7295));
#1739=EDGE_LOOP('',(#7296,#7297,#7298,#7299));
#1740=EDGE_LOOP('',(#7300,#7301,#7302,#7303));
#1741=EDGE_LOOP('',(#7304,#7305,#7306,#7307,#7308));
#1742=EDGE_LOOP('',(#7309,#7310,#7311,#7312));
#1743=EDGE_LOOP('',(#7313,#7314,#7315,#7316));
#1744=EDGE_LOOP('',(#7317));
#1745=EDGE_LOOP('',(#7318,#7319,#7320,#7321));
#1746=EDGE_LOOP('',(#7322,#7323,#7324,#7325,#7326,#7327,#7328,#7329,#7330,
#7331));
#1747=EDGE_LOOP('',(#7332));
#1748=EDGE_LOOP('',(#7333));
#1749=EDGE_LOOP('',(#7334,#7335,#7336,#7337,#7338));
#1750=EDGE_LOOP('',(#7339));
#1751=EDGE_LOOP('',(#7340));
#1752=EDGE_LOOP('',(#7341,#7342,#7343,#7344));
#1753=EDGE_LOOP('',(#7345));
#1754=EDGE_LOOP('',(#7346));
#1755=EDGE_LOOP('',(#7347));
#1756=EDGE_LOOP('',(#7348));
#1757=EDGE_LOOP('',(#7349));
#1758=EDGE_LOOP('',(#7350,#7351,#7352,#7353));
#1759=EDGE_LOOP('',(#7354));
#1760=EDGE_LOOP('',(#7355));
#1761=EDGE_LOOP('',(#7356));
#1762=EDGE_LOOP('',(#7357,#7358,#7359,#7360,#7361,#7362,#7363,#7364));
#1763=EDGE_LOOP('',(#7365,#7366,#7367,#7368));
#1764=EDGE_LOOP('',(#7369,#7370,#7371,#7372));
#1765=EDGE_LOOP('',(#7373,#7374,#7375,#7376,#7377,#7378,#7379,#7380,#7381,
#7382));
#1766=EDGE_LOOP('',(#7383));
#1767=EDGE_LOOP('',(#7384,#7385,#7386,#7387));
#1768=EDGE_LOOP('',(#7388));
#1769=EDGE_LOOP('',(#7389,#7390,#7391,#7392));
#1770=EDGE_LOOP('',(#7393,#7394,#7395,#7396));
#1771=EDGE_LOOP('',(#7397,#7398,#7399,#7400));
#1772=EDGE_LOOP('',(#7401));
#1773=EDGE_LOOP('',(#7402));
#1774=EDGE_LOOP('',(#7403,#7404,#7405,#7406));
#1775=EDGE_LOOP('',(#7407,#7408,#7409,#7410));
#1776=EDGE_LOOP('',(#7411));
#1777=EDGE_LOOP('',(#7412,#7413,#7414,#7415,#7416,#7417,#7418,#7419,#7420,
#7421,#7422,#7423));
#1778=EDGE_LOOP('',(#7424));
#1779=EDGE_LOOP('',(#7425,#7426,#7427,#7428,#7429));
#1780=EDGE_LOOP('',(#7430,#7431,#7432,#7433));
#1781=EDGE_LOOP('',(#7434,#7435,#7436,#7437));
#1782=EDGE_LOOP('',(#7438,#7439,#7440,#7441));
#1783=EDGE_LOOP('',(#7442,#7443,#7444,#7445));
#1784=EDGE_LOOP('',(#7446,#7447,#7448,#7449));
#1785=EDGE_LOOP('',(#7450,#7451,#7452,#7453,#7454,#7455,#7456,#7457,#7458,
#7459,#7460,#7461,#7462,#7463,#7464,#7465,#7466,#7467,#7468,#7469));
#1786=EDGE_LOOP('',(#7470));
#1787=EDGE_LOOP('',(#7471,#7472,#7473,#7474,#7475,#7476,#7477,#7478,#7479,
#7480,#7481,#7482,#7483,#7484,#7485,#7486,#7487,#7488,#7489,#7490));
#1788=EDGE_LOOP('',(#7491));
#1789=EDGE_LOOP('',(#7492,#7493,#7494,#7495,#7496));
#1790=EDGE_LOOP('',(#7497,#7498,#7499,#7500));
#1791=EDGE_LOOP('',(#7501,#7502,#7503,#7504));
#1792=EDGE_LOOP('',(#7505,#7506,#7507,#7508));
#1793=EDGE_LOOP('',(#7509,#7510,#7511,#7512));
#1794=EDGE_LOOP('',(#7513,#7514,#7515,#7516));
#1795=EDGE_LOOP('',(#7517,#7518,#7519,#7520));
#1796=EDGE_LOOP('',(#7521,#7522,#7523,#7524));
#1797=EDGE_LOOP('',(#7525,#7526,#7527,#7528));
#1798=EDGE_LOOP('',(#7529,#7530,#7531,#7532));
#1799=EDGE_LOOP('',(#7533,#7534,#7535,#7536));
#1800=EDGE_LOOP('',(#7537,#7538,#7539,#7540));
#1801=EDGE_LOOP('',(#7541,#7542,#7543,#7544));
#1802=EDGE_LOOP('',(#7545,#7546,#7547,#7548));
#1803=EDGE_LOOP('',(#7549,#7550,#7551,#7552));
#1804=EDGE_LOOP('',(#7553,#7554,#7555,#7556));
#1805=EDGE_LOOP('',(#7557,#7558,#7559,#7560));
#1806=EDGE_LOOP('',(#7561,#7562,#7563,#7564,#7565));
#1807=EDGE_LOOP('',(#7566,#7567,#7568,#7569));
#1808=EDGE_LOOP('',(#7570,#7571,#7572,#7573,#7574));
#1809=EDGE_LOOP('',(#7575));
#1810=EDGE_LOOP('',(#7576));
#1811=EDGE_LOOP('',(#7577,#7578,#7579,#7580,#7581));
#1812=EDGE_LOOP('',(#7582,#7583,#7584,#7585));
#1813=EDGE_LOOP('',(#7586));
#1814=EDGE_LOOP('',(#7587,#7588,#7589,#7590,#7591));
#1815=EDGE_LOOP('',(#7592,#7593));
#1816=EDGE_LOOP('',(#7594));
#1817=EDGE_LOOP('',(#7595));
#1818=EDGE_LOOP('',(#7596,#7597,#7598,#7599,#7600));
#1819=EDGE_LOOP('',(#7601));
#1820=EDGE_LOOP('',(#7602,#7603,#7604,#7605,#7606,#7607,#7608,#7609));
#1821=EDGE_LOOP('',(#7610,#7611,#7612,#7613));
#1822=EDGE_LOOP('',(#7614,#7615,#7616,#7617));
#1823=EDGE_LOOP('',(#7618,#7619,#7620,#7621));
#1824=EDGE_LOOP('',(#7622,#7623,#7624,#7625));
#1825=EDGE_LOOP('',(#7626,#7627,#7628,#7629,#7630,#7631,#7632,#7633));
#1826=EDGE_LOOP('',(#7634,#7635,#7636,#7637,#7638));
#1827=EDGE_LOOP('',(#7639));
#1828=EDGE_LOOP('',(#7640,#7641,#7642,#7643,#7644));
#1829=EDGE_LOOP('',(#7645,#7646,#7647,#7648,#7649));
#1830=EDGE_LOOP('',(#7650,#7651,#7652,#7653));
#1831=EDGE_LOOP('',(#7654,#7655,#7656,#7657));
#1832=EDGE_LOOP('',(#7658,#7659,#7660,#7661));
#1833=EDGE_LOOP('',(#7662,#7663,#7664,#7665));
#1834=EDGE_LOOP('',(#7666,#7667,#7668,#7669,#7670));
#1835=EDGE_LOOP('',(#7671,#7672,#7673,#7674,#7675));
#1836=EDGE_LOOP('',(#7676,#7677,#7678,#7679,#7680));
#1837=EDGE_LOOP('',(#7681,#7682,#7683,#7684,#7685));
#1838=EDGE_LOOP('',(#7686,#7687,#7688,#7689));
#1839=EDGE_LOOP('',(#7690,#7691,#7692,#7693));
#1840=EDGE_LOOP('',(#7694,#7695,#7696,#7697,#7698));
#1841=EDGE_LOOP('',(#7699,#7700,#7701,#7702,#7703));
#1842=EDGE_LOOP('',(#7704,#7705,#7706,#7707,#7708));
#1843=EDGE_LOOP('',(#7709,#7710,#7711,#7712,#7713));
#1844=EDGE_LOOP('',(#7714,#7715,#7716,#7717));
#1845=EDGE_LOOP('',(#7718,#7719,#7720,#7721));
#1846=EDGE_LOOP('',(#7722,#7723));
#1847=EDGE_LOOP('',(#7724,#7725,#7726,#7727));
#1848=EDGE_LOOP('',(#7728,#7729,#7730,#7731,#7732,#7733,#7734,#7735,#7736,
#7737,#7738,#7739));
#1849=EDGE_LOOP('',(#7740,#7741,#7742,#7743));
#1850=EDGE_LOOP('',(#7744,#7745,#7746,#7747));
#1851=EDGE_LOOP('',(#7748,#7749,#7750,#7751));
#1852=EDGE_LOOP('',(#7752,#7753,#7754,#7755));
#1853=EDGE_LOOP('',(#7756,#7757,#7758,#7759));
#1854=EDGE_LOOP('',(#7760,#7761,#7762,#7763));
#1855=EDGE_LOOP('',(#7764,#7765,#7766,#7767));
#1856=EDGE_LOOP('',(#7768,#7769,#7770,#7771));
#1857=EDGE_LOOP('',(#7772,#7773,#7774,#7775));
#1858=EDGE_LOOP('',(#7776,#7777,#7778,#7779,#7780,#7781,#7782,#7783,#7784,
#7785));
#1859=EDGE_LOOP('',(#7786,#7787));
#1860=EDGE_LOOP('',(#7788,#7789,#7790,#7791,#7792,#7793,#7794,#7795,#7796,
#7797));
#1861=EDGE_LOOP('',(#7798));
#1862=EDGE_LOOP('',(#7799));
#1863=EDGE_LOOP('',(#7800));
#1864=EDGE_LOOP('',(#7801));
#1865=EDGE_LOOP('',(#7802));
#1866=EDGE_LOOP('',(#7803,#7804,#7805,#7806,#7807,#7808,#7809,#7810,#7811,
#7812,#7813,#7814,#7815,#7816,#7817,#7818,#7819));
#1867=EDGE_LOOP('',(#7820,#7821));
#1868=EDGE_LOOP('',(#7822,#7823));
#1869=EDGE_LOOP('',(#7824,#7825,#7826,#7827,#7828,#7829,#7830,#7831));
#1870=EDGE_LOOP('',(#7832,#7833,#7834,#7835,#7836,#7837,#7838,#7839));
#1871=EDGE_LOOP('',(#7840,#7841,#7842,#7843,#7844,#7845,#7846,#7847));
#1872=EDGE_LOOP('',(#7848,#7849,#7850,#7851,#7852,#7853));
#1873=EDGE_LOOP('',(#7854,#7855,#7856,#7857));
#1874=EDGE_LOOP('',(#7858,#7859,#7860,#7861));
#1875=EDGE_LOOP('',(#7862,#7863));
#1876=EDGE_LOOP('',(#7864,#7865,#7866,#7867));
#1877=EDGE_LOOP('',(#7868,#7869));
#1878=EDGE_LOOP('',(#7870,#7871));
#1879=EDGE_LOOP('',(#7872,#7873,#7874,#7875));
#1880=EDGE_LOOP('',(#7876,#7877));
#1881=EDGE_LOOP('',(#7878,#7879));
#1882=EDGE_LOOP('',(#7880,#7881,#7882,#7883));
#1883=EDGE_LOOP('',(#7884,#7885));
#1884=EDGE_LOOP('',(#7886,#7887));
#1885=EDGE_LOOP('',(#7888,#7889,#7890,#7891));
#1886=EDGE_LOOP('',(#7892,#7893));
#1887=EDGE_LOOP('',(#7894,#7895));
#1888=EDGE_LOOP('',(#7896,#7897,#7898,#7899));
#1889=EDGE_LOOP('',(#7900,#7901));
#1890=EDGE_LOOP('',(#7902,#7903,#7904));
#1891=EDGE_LOOP('',(#7905,#7906,#7907,#7908));
#1892=EDGE_LOOP('',(#7909,#7910,#7911));
#1893=EDGE_LOOP('',(#7912,#7913));
#1894=EDGE_LOOP('',(#7914,#7915,#7916,#7917));
#1895=EDGE_LOOP('',(#7918,#7919));
#1896=EDGE_LOOP('',(#7920,#7921));
#1897=EDGE_LOOP('',(#7922,#7923,#7924,#7925));
#1898=EDGE_LOOP('',(#7926,#7927));
#1899=EDGE_LOOP('',(#7928,#7929));
#1900=EDGE_LOOP('',(#7930,#7931,#7932,#7933));
#1901=EDGE_LOOP('',(#7934,#7935));
#1902=EDGE_LOOP('',(#7936,#7937));
#1903=EDGE_LOOP('',(#7938,#7939,#7940,#7941));
#1904=EDGE_LOOP('',(#7942,#7943));
#1905=EDGE_LOOP('',(#7944,#7945,#7946,#7947,#7948,#7949,#7950));
#1906=EDGE_LOOP('',(#7951,#7952,#7953,#7954,#7955));
#1907=EDGE_LOOP('',(#7956,#7957,#7958,#7959));
#1908=EDGE_LOOP('',(#7960,#7961,#7962,#7963,#7964));
#1909=EDGE_LOOP('',(#7965,#7966,#7967,#7968));
#1910=EDGE_LOOP('',(#7969,#7970,#7971,#7972,#7973));
#1911=EDGE_LOOP('',(#7974,#7975,#7976,#7977,#7978,#7979,#7980,#7981,#7982,
#7983));
#1912=EDGE_LOOP('',(#7984,#7985));
#1913=EDGE_LOOP('',(#7986));
#1914=EDGE_LOOP('',(#7987));
#1915=EDGE_LOOP('',(#7988));
#1916=EDGE_LOOP('',(#7989));
#1917=EDGE_LOOP('',(#7990,#7991,#7992,#7993,#7994,#7995,#7996));
#1918=EDGE_LOOP('',(#7997));
#1919=EDGE_LOOP('',(#7998,#7999,#8000,#8001,#8002));
#1920=EDGE_LOOP('',(#8003));
#1921=EDGE_LOOP('',(#8004,#8005,#8006,#8007));
#1922=EDGE_LOOP('',(#8008));
#1923=EDGE_LOOP('',(#8009));
#1924=EDGE_LOOP('',(#8010,#8011,#8012,#8013));
#1925=EDGE_LOOP('',(#8014));
#1926=EDGE_LOOP('',(#8015));
#1927=EDGE_LOOP('',(#8016,#8017,#8018));
#1928=EDGE_LOOP('',(#8019,#8020,#8021,#8022));
#1929=EDGE_LOOP('',(#8023,#8024,#8025,#8026));
#1930=EDGE_LOOP('',(#8027,#8028,#8029,#8030));
#1931=EDGE_LOOP('',(#8031,#8032,#8033,#8034,#8035,#8036));
#1932=EDGE_LOOP('',(#8037,#8038,#8039,#8040));
#1933=EDGE_LOOP('',(#8041,#8042,#8043,#8044));
#1934=EDGE_LOOP('',(#8045,#8046,#8047,#8048));
#1935=EDGE_LOOP('',(#8049,#8050,#8051,#8052));
#1936=EDGE_LOOP('',(#8053,#8054,#8055,#8056));
#1937=EDGE_LOOP('',(#8057,#8058,#8059,#8060));
#1938=EDGE_LOOP('',(#8061));
#1939=EDGE_LOOP('',(#8062,#8063,#8064,#8065,#8066,#8067));
#1940=EDGE_LOOP('',(#8068,#8069));
#1941=EDGE_LOOP('',(#8070,#8071));
#1942=EDGE_LOOP('',(#8072,#8073,#8074,#8075,#8076,#8077));
#1943=EDGE_LOOP('',(#8078,#8079));
#1944=EDGE_LOOP('',(#8080,#8081));
#1945=EDGE_LOOP('',(#8082,#8083,#8084,#8085,#8086));
#1946=EDGE_LOOP('',(#8087));
#1947=EDGE_LOOP('',(#8088));
#1948=EDGE_LOOP('',(#8089));
#1949=EDGE_LOOP('',(#8090));
#1950=EDGE_LOOP('',(#8091,#8092,#8093,#8094));
#1951=EDGE_LOOP('',(#8095));
#1952=EDGE_LOOP('',(#8096,#8097,#8098,#8099));
#1953=EDGE_LOOP('',(#8100,#8101,#8102,#8103));
#1954=EDGE_LOOP('',(#8104,#8105,#8106,#8107));
#1955=EDGE_LOOP('',(#8108,#8109,#8110,#8111));
#1956=EDGE_LOOP('',(#8112,#8113,#8114,#8115));
#1957=EDGE_LOOP('',(#8116,#8117,#8118,#8119));
#1958=EDGE_LOOP('',(#8120,#8121,#8122,#8123,#8124));
#1959=EDGE_LOOP('',(#8125));
#1960=EDGE_LOOP('',(#8126,#8127,#8128,#8129));
#1961=EDGE_LOOP('',(#8130,#8131,#8132,#8133,#8134,#8135,#8136,#8137,#8138,
#8139,#8140,#8141));
#1962=EDGE_LOOP('',(#8142,#8143,#8144,#8145));
#1963=EDGE_LOOP('',(#8146,#8147,#8148,#8149));
#1964=EDGE_LOOP('',(#8150,#8151,#8152,#8153));
#1965=EDGE_LOOP('',(#8154,#8155,#8156,#8157));
#1966=EDGE_LOOP('',(#8158,#8159,#8160,#8161));
#1967=EDGE_LOOP('',(#8162,#8163,#8164,#8165,#8166,#8167,#8168,#8169,#8170,
#8171,#8172,#8173));
#1968=EDGE_LOOP('',(#8174,#8175,#8176,#8177));
#1969=EDGE_LOOP('',(#8178,#8179,#8180,#8181));
#1970=EDGE_LOOP('',(#8182,#8183,#8184,#8185));
#1971=EDGE_LOOP('',(#8186,#8187,#8188,#8189));
#1972=EDGE_LOOP('',(#8190,#8191,#8192,#8193));
#1973=EDGE_LOOP('',(#8194,#8195,#8196,#8197));
#1974=EDGE_LOOP('',(#8198,#8199,#8200,#8201));
#1975=EDGE_LOOP('',(#8202,#8203,#8204,#8205));
#1976=EDGE_LOOP('',(#8206,#8207,#8208,#8209));
#1977=EDGE_LOOP('',(#8210,#8211,#8212,#8213));
#1978=EDGE_LOOP('',(#8214,#8215,#8216,#8217));
#1979=EDGE_LOOP('',(#8218,#8219,#8220,#8221));
#1980=EDGE_LOOP('',(#8222,#8223,#8224,#8225,#8226,#8227,#8228,#8229,#8230,
#8231,#8232,#8233));
#1981=EDGE_LOOP('',(#8234,#8235,#8236,#8237));
#1982=EDGE_LOOP('',(#8238,#8239,#8240,#8241));
#1983=EDGE_LOOP('',(#8242,#8243,#8244,#8245));
#1984=EDGE_LOOP('',(#8246,#8247,#8248,#8249));
#1985=EDGE_LOOP('',(#8250,#8251,#8252,#8253));
#1986=EDGE_LOOP('',(#8254,#8255,#8256,#8257));
#1987=EDGE_LOOP('',(#8258,#8259,#8260,#8261));
#1988=EDGE_LOOP('',(#8262,#8263,#8264,#8265));
#1989=EDGE_LOOP('',(#8266,#8267,#8268,#8269));
#1990=EDGE_LOOP('',(#8270,#8271,#8272,#8273));
#1991=EDGE_LOOP('',(#8274,#8275,#8276,#8277));
#1992=EDGE_LOOP('',(#8278,#8279,#8280,#8281));
#1993=EDGE_LOOP('',(#8282,#8283,#8284,#8285,#8286,#8287,#8288,#8289,#8290,
#8291,#8292,#8293));
#1994=EDGE_LOOP('',(#8294,#8295,#8296,#8297));
#1995=EDGE_LOOP('',(#8298));
#1996=EDGE_LOOP('',(#8299));
#1997=EDGE_LOOP('',(#8300,#8301,#8302,#8303));
#1998=EDGE_LOOP('',(#8304));
#1999=EDGE_LOOP('',(#8305));
#2000=EDGE_LOOP('',(#8306));
#2001=EDGE_LOOP('',(#8307));
#2002=EDGE_LOOP('',(#8308));
#2003=EDGE_LOOP('',(#8309));
#2004=EDGE_LOOP('',(#8310,#8311,#8312,#8313));
#2005=EDGE_LOOP('',(#8314,#8315,#8316,#8317));
#2006=EDGE_LOOP('',(#8318,#8319,#8320,#8321));
#2007=EDGE_LOOP('',(#8322));
#2008=EDGE_LOOP('',(#8323));
#2009=EDGE_LOOP('',(#8324,#8325,#8326,#8327));
#2010=EDGE_LOOP('',(#8328));
#2011=EDGE_LOOP('',(#8329));
#2012=EDGE_LOOP('',(#8330));
#2013=EDGE_LOOP('',(#8331,#8332,#8333,#8334));
#2014=EDGE_LOOP('',(#8335));
#2015=EDGE_LOOP('',(#8336));
#2016=EDGE_LOOP('',(#8337));
#2017=EDGE_LOOP('',(#8338,#8339,#8340,#8341));
#2018=EDGE_LOOP('',(#8342,#8343,#8344,#8345,#8346,#8347,#8348,#8349));
#2019=EDGE_LOOP('',(#8350,#8351,#8352,#8353,#8354,#8355,#8356,#8357));
#2020=EDGE_LOOP('',(#8358,#8359,#8360,#8361,#8362,#8363,#8364,#8365));
#2021=EDGE_LOOP('',(#8366,#8367,#8368,#8369,#8370,#8371,#8372,#8373,#8374));
#2022=EDGE_LOOP('',(#8375,#8376,#8377,#8378,#8379,#8380,#8381,#8382));
#2023=EDGE_LOOP('',(#8383,#8384,#8385,#8386,#8387,#8388,#8389,#8390));
#2024=EDGE_LOOP('',(#8391,#8392,#8393,#8394,#8395,#8396,#8397,#8398));
#2025=EDGE_LOOP('',(#8399,#8400,#8401,#8402,#8403,#8404,#8405,#8406));
#2026=EDGE_LOOP('',(#8407,#8408,#8409,#8410,#8411,#8412,#8413,#8414));
#2027=EDGE_LOOP('',(#8415,#8416,#8417,#8418,#8419,#8420,#8421,#8422,#8423,
#8424,#8425,#8426,#8427,#8428,#8429,#8430,#8431,#8432,#8433,#8434));
#2028=EDGE_LOOP('',(#8435));
#2029=EDGE_LOOP('',(#8436,#8437,#8438,#8439));
#2030=EDGE_LOOP('',(#8440,#8441,#8442,#8443));
#2031=EDGE_LOOP('',(#8444,#8445,#8446,#8447,#8448,#8449,#8450,#8451));
#2032=EDGE_LOOP('',(#8452));
#2033=EDGE_LOOP('',(#8453));
#2034=EDGE_LOOP('',(#8454,#8455,#8456,#8457,#8458));
#2035=EDGE_LOOP('',(#8459,#8460,#8461,#8462,#8463));
#2036=EDGE_LOOP('',(#8464,#8465));
#2037=EDGE_LOOP('',(#8466,#8467));
#2038=EDGE_LOOP('',(#8468,#8469));
#2039=EDGE_LOOP('',(#8470,#8471));
#2040=EDGE_LOOP('',(#8472,#8473));
#2041=EDGE_LOOP('',(#8474));
#2042=EDGE_LOOP('',(#8475));
#2043=EDGE_LOOP('',(#8476,#8477,#8478,#8479,#8480));
#2044=EDGE_LOOP('',(#8481,#8482,#8483,#8484,#8485,#8486,#8487,#8488,#8489,
#8490,#8491,#8492,#8493,#8494,#8495,#8496,#8497,#8498,#8499,#8500,#8501,
#8502,#8503,#8504,#8505));
#2045=EDGE_LOOP('',(#8506));
#2046=EDGE_LOOP('',(#8507));
#2047=EDGE_LOOP('',(#8508,#8509,#8510,#8511));
#2048=EDGE_LOOP('',(#8512,#8513));
#2049=EDGE_LOOP('',(#8514,#8515));
#2050=EDGE_LOOP('',(#8516,#8517));
#2051=EDGE_LOOP('',(#8518,#8519));
#2052=EDGE_LOOP('',(#8520,#8521));
#2053=EDGE_LOOP('',(#8522,#8523,#8524,#8525,#8526,#8527));
#2054=EDGE_LOOP('',(#8528,#8529,#8530,#8531,#8532,#8533));
#2055=EDGE_LOOP('',(#8534,#8535,#8536,#8537,#8538,#8539));
#2056=EDGE_LOOP('',(#8540,#8541,#8542,#8543,#8544,#8545));
#2057=EDGE_LOOP('',(#8546,#8547,#8548,#8549,#8550,#8551));
#2058=EDGE_LOOP('',(#8552,#8553,#8554,#8555));
#2059=EDGE_LOOP('',(#8556,#8557,#8558,#8559));
#2060=EDGE_LOOP('',(#8560));
#2061=EDGE_LOOP('',(#8561));
#2062=EDGE_LOOP('',(#8562,#8563,#8564,#8565));
#2063=EDGE_LOOP('',(#8566));
#2064=EDGE_LOOP('',(#8567));
#2065=EDGE_LOOP('',(#8568,#8569,#8570,#8571));
#2066=EDGE_LOOP('',(#8572,#8573,#8574,#8575));
#2067=EDGE_LOOP('',(#8576,#8577,#8578,#8579));
#2068=EDGE_LOOP('',(#8580,#8581,#8582,#8583));
#2069=EDGE_LOOP('',(#8584,#8585,#8586,#8587));
#2070=EDGE_LOOP('',(#8588,#8589,#8590,#8591));
#2071=EDGE_LOOP('',(#8592,#8593,#8594,#8595));
#2072=EDGE_LOOP('',(#8596,#8597,#8598,#8599));
#2073=EDGE_LOOP('',(#8600,#8601,#8602,#8603));
#2074=EDGE_LOOP('',(#8604,#8605,#8606,#8607));
#2075=EDGE_LOOP('',(#8608,#8609,#8610,#8611,#8612,#8613));
#2076=EDGE_LOOP('',(#8614,#8615,#8616,#8617));
#2077=EDGE_LOOP('',(#8618,#8619,#8620,#8621));
#2078=EDGE_LOOP('',(#8622,#8623,#8624,#8625,#8626,#8627));
#2079=EDGE_LOOP('',(#8628,#8629,#8630,#8631,#8632,#8633));
#2080=EDGE_LOOP('',(#8634,#8635,#8636,#8637));
#2081=EDGE_LOOP('',(#8638,#8639,#8640,#8641));
#2082=EDGE_LOOP('',(#8642,#8643,#8644,#8645,#8646,#8647));
#2083=EDGE_LOOP('',(#8648,#8649,#8650,#8651,#8652,#8653));
#2084=EDGE_LOOP('',(#8654,#8655,#8656,#8657));
#2085=EDGE_LOOP('',(#8658,#8659,#8660,#8661));
#2086=EDGE_LOOP('',(#8662,#8663,#8664,#8665,#8666,#8667));
#2087=EDGE_LOOP('',(#8668,#8669,#8670,#8671,#8672,#8673));
#2088=EDGE_LOOP('',(#8674,#8675,#8676,#8677));
#2089=EDGE_LOOP('',(#8678,#8679,#8680,#8681));
#2090=EDGE_LOOP('',(#8682,#8683,#8684,#8685,#8686,#8687));
#2091=EDGE_LOOP('',(#8688,#8689,#8690,#8691,#8692,#8693));
#2092=EDGE_LOOP('',(#8694,#8695,#8696,#8697));
#2093=EDGE_LOOP('',(#8698,#8699,#8700,#8701));
#2094=EDGE_LOOP('',(#8702,#8703,#8704,#8705,#8706,#8707));
#2095=EDGE_LOOP('',(#8708,#8709,#8710,#8711,#8712,#8713));
#2096=EDGE_LOOP('',(#8714,#8715,#8716,#8717));
#2097=EDGE_LOOP('',(#8718,#8719,#8720,#8721));
#2098=EDGE_LOOP('',(#8722,#8723,#8724,#8725,#8726,#8727));
#2099=EDGE_LOOP('',(#8728,#8729,#8730,#8731,#8732,#8733));
#2100=EDGE_LOOP('',(#8734,#8735,#8736,#8737));
#2101=EDGE_LOOP('',(#8738,#8739,#8740,#8741));
#2102=EDGE_LOOP('',(#8742,#8743,#8744,#8745,#8746,#8747));
#2103=EDGE_LOOP('',(#8748,#8749,#8750,#8751,#8752,#8753));
#2104=EDGE_LOOP('',(#8754,#8755,#8756,#8757));
#2105=EDGE_LOOP('',(#8758,#8759,#8760,#8761));
#2106=EDGE_LOOP('',(#8762,#8763,#8764,#8765,#8766,#8767));
#2107=EDGE_LOOP('',(#8768,#8769,#8770,#8771,#8772,#8773));
#2108=EDGE_LOOP('',(#8774,#8775,#8776,#8777));
#2109=EDGE_LOOP('',(#8778,#8779,#8780,#8781));
#2110=EDGE_LOOP('',(#8782,#8783,#8784,#8785,#8786,#8787));
#2111=EDGE_LOOP('',(#8788,#8789,#8790,#8791,#8792,#8793));
#2112=EDGE_LOOP('',(#8794,#8795,#8796,#8797));
#2113=EDGE_LOOP('',(#8798,#8799,#8800,#8801));
#2114=EDGE_LOOP('',(#8802,#8803,#8804,#8805,#8806,#8807));
#2115=EDGE_LOOP('',(#8808));
#2116=EDGE_LOOP('',(#8809));
#2117=EDGE_LOOP('',(#8810));
#2118=EDGE_LOOP('',(#8811,#8812,#8813,#8814,#8815,#8816,#8817,#8818,#8819,
#8820,#8821,#8822,#8823,#8824,#8825,#8826,#8827,#8828,#8829,#8830,#8831,
#8832,#8833,#8834));
#2119=EDGE_LOOP('',(#8835,#8836,#8837,#8838));
#2120=EDGE_LOOP('',(#8839,#8840,#8841,#8842));
#2121=EDGE_LOOP('',(#8843,#8844,#8845,#8846));
#2122=EDGE_LOOP('',(#8847,#8848,#8849,#8850));
#2123=EDGE_LOOP('',(#8851,#8852,#8853,#8854));
#2124=EDGE_LOOP('',(#8855,#8856,#8857,#8858));
#2125=EDGE_LOOP('',(#8859,#8860,#8861,#8862,#8863));
#2126=EDGE_LOOP('',(#8864,#8865,#8866,#8867,#8868));
#2127=EDGE_LOOP('',(#8869,#8870,#8871,#8872,#8873,#8874,#8875,#8876,#8877,
#8878,#8879,#8880,#8881,#8882,#8883,#8884,#8885,#8886,#8887,#8888,#8889,
#8890,#8891,#8892));
#2128=EDGE_LOOP('',(#8893));
#2129=EDGE_LOOP('',(#8894,#8895,#8896,#8897));
#2130=EDGE_LOOP('',(#8898,#8899,#8900,#8901));
#2131=EDGE_LOOP('',(#8902,#8903,#8904,#8905));
#2132=EDGE_LOOP('',(#8906,#8907,#8908,#8909));
#2133=EDGE_LOOP('',(#8910,#8911,#8912,#8913));
#2134=EDGE_LOOP('',(#8914,#8915,#8916,#8917));
#2135=EDGE_LOOP('',(#8918,#8919,#8920,#8921));
#2136=EDGE_LOOP('',(#8922,#8923,#8924,#8925));
#2137=EDGE_LOOP('',(#8926,#8927,#8928,#8929));
#2138=EDGE_LOOP('',(#8930,#8931,#8932,#8933));
#2139=EDGE_LOOP('',(#8934,#8935,#8936,#8937));
#2140=EDGE_LOOP('',(#8938,#8939,#8940,#8941));
#2141=EDGE_LOOP('',(#8942,#8943,#8944,#8945));
#2142=EDGE_LOOP('',(#8946,#8947,#8948,#8949));
#2143=EDGE_LOOP('',(#8950,#8951,#8952,#8953));
#2144=EDGE_LOOP('',(#8954,#8955,#8956,#8957));
#2145=EDGE_LOOP('',(#8958,#8959,#8960,#8961));
#2146=EDGE_LOOP('',(#8962,#8963,#8964,#8965));
#2147=EDGE_LOOP('',(#8966,#8967,#8968,#8969,#8970));
#2148=EDGE_LOOP('',(#8971,#8972,#8973,#8974,#8975));
#2149=EDGE_LOOP('',(#8976,#8977,#8978,#8979));
#2150=EDGE_LOOP('',(#8980,#8981,#8982,#8983,#8984));
#2151=EDGE_LOOP('',(#8985,#8986,#8987,#8988,#8989));
#2152=EDGE_LOOP('',(#8990,#8991,#8992,#8993,#8994));
#2153=EDGE_LOOP('',(#8995,#8996,#8997,#8998,#8999));
#2154=EDGE_LOOP('',(#9000,#9001,#9002,#9003));
#2155=EDGE_LOOP('',(#9004,#9005,#9006,#9007));
#2156=EDGE_LOOP('',(#9008));
#2157=EDGE_LOOP('',(#9009));
#2158=EDGE_LOOP('',(#9010,#9011,#9012,#9013));
#2159=EDGE_LOOP('',(#9014,#9015,#9016,#9017));
#2160=EDGE_LOOP('',(#9018,#9019,#9020,#9021));
#2161=EDGE_LOOP('',(#9022));
#2162=EDGE_LOOP('',(#9023));
#2163=EDGE_LOOP('',(#9024,#9025,#9026,#9027));
#2164=EDGE_LOOP('',(#9028));
#2165=EDGE_LOOP('',(#9029));
#2166=EDGE_LOOP('',(#9030,#9031,#9032,#9033,#9034));
#2167=EDGE_LOOP('',(#9035,#9036,#9037,#9038,#9039,#9040));
#2168=EDGE_LOOP('',(#9041,#9042,#9043,#9044,#9045,#9046));
#2169=EDGE_LOOP('',(#9047,#9048,#9049,#9050,#9051,#9052));
#2170=EDGE_LOOP('',(#9053,#9054,#9055,#9056,#9057));
#2171=EDGE_LOOP('',(#9058));
#2172=EDGE_LOOP('',(#9059));
#2173=EDGE_LOOP('',(#9060,#9061,#9062,#9063));
#2174=EDGE_LOOP('',(#9064,#9065));
#2175=EDGE_LOOP('',(#9066));
#2176=EDGE_LOOP('',(#9067,#9068,#9069,#9070));
#2177=EDGE_LOOP('',(#9071,#9072,#9073,#9074,#9075));
#2178=EDGE_LOOP('',(#9076));
#2179=EDGE_LOOP('',(#9077));
#2180=EDGE_LOOP('',(#9078,#9079,#9080,#9081,#9082));
#2181=EDGE_LOOP('',(#9083,#9084,#9085,#9086,#9087));
#2182=EDGE_LOOP('',(#9088,#9089,#9090,#9091,#9092));
#2183=EDGE_LOOP('',(#9093));
#2184=EDGE_LOOP('',(#9094,#9095,#9096,#9097));
#2185=EDGE_LOOP('',(#9098,#9099,#9100,#9101));
#2186=EDGE_LOOP('',(#9102));
#2187=EDGE_LOOP('',(#9103));
#2188=EDGE_LOOP('',(#9104,#9105,#9106,#9107));
#2189=EDGE_LOOP('',(#9108,#9109,#9110,#9111,#9112,#9113,#9114,#9115,#9116,
#9117,#9118,#9119));
#2190=EDGE_LOOP('',(#9120));
#2191=EDGE_LOOP('',(#9121,#9122,#9123,#9124,#9125,#9126,#9127,#9128,#9129,
#9130,#9131,#9132));
#2192=EDGE_LOOP('',(#9133));
#2193=EDGE_LOOP('',(#9134,#9135,#9136,#9137,#9138,#9139,#9140,#9141));
#2194=EDGE_LOOP('',(#9142,#9143,#9144,#9145,#9146,#9147,#9148,#9149));
#2195=EDGE_LOOP('',(#9150,#9151,#9152,#9153,#9154,#9155,#9156,#9157));
#2196=EDGE_LOOP('',(#9158,#9159,#9160,#9161,#9162,#9163,#9164,#9165));
#2197=EDGE_LOOP('',(#9166,#9167,#9168,#9169,#9170,#9171,#9172,#9173));
#2198=EDGE_LOOP('',(#9174,#9175,#9176,#9177,#9178,#9179,#9180,#9181));
#2199=EDGE_LOOP('',(#9182,#9183,#9184));
#2200=EDGE_LOOP('',(#9185,#9186,#9187));
#2201=EDGE_LOOP('',(#9188,#9189,#9190));
#2202=EDGE_LOOP('',(#9191,#9192,#9193));
#2203=EDGE_LOOP('',(#9194,#9195,#9196));
#2204=EDGE_LOOP('',(#9197,#9198,#9199));
#2205=EDGE_LOOP('',(#9200,#9201,#9202));
#2206=EDGE_LOOP('',(#9203,#9204,#9205));
#2207=EDGE_LOOP('',(#9206,#9207,#9208));
#2208=EDGE_LOOP('',(#9209,#9210,#9211));
#2209=EDGE_LOOP('',(#9212,#9213,#9214));
#2210=EDGE_LOOP('',(#9215,#9216,#9217));
#2211=EDGE_LOOP('',(#9218,#9219,#9220,#9221));
#2212=CIRCLE('',#10270,18.);
#2213=CIRCLE('',#10271,18.);
#2214=CIRCLE('',#10273,18.);
#2215=CIRCLE('',#10274,18.);
#2216=CIRCLE('',#10276,18.);
#2217=CIRCLE('',#10277,18.);
#2218=CIRCLE('',#10279,18.);
#2219=CIRCLE('',#10280,18.);
#2220=CIRCLE('',#10282,18.);
#2221=CIRCLE('',#10283,18.);
#2222=CIRCLE('',#10285,18.);
#2223=CIRCLE('',#10286,18.);
#2224=CIRCLE('',#10288,18.);
#2225=CIRCLE('',#10289,18.);
#2226=CIRCLE('',#10291,18.);
#2227=CIRCLE('',#10292,18.);
#2228=CIRCLE('',#10294,18.);
#2229=CIRCLE('',#10295,18.);
#2230=CIRCLE('',#10297,18.);
#2231=CIRCLE('',#10298,18.);
#2232=CIRCLE('',#10300,18.);
#2233=CIRCLE('',#10301,18.);
#2234=CIRCLE('',#10303,18.);
#2235=CIRCLE('',#10304,18.);
#2236=CIRCLE('',#10306,18.);
#2237=CIRCLE('',#10307,18.);
#2238=CIRCLE('',#10309,18.);
#2239=CIRCLE('',#10310,18.);
#2240=CIRCLE('',#10312,18.);
#2241=CIRCLE('',#10313,18.);
#2242=CIRCLE('',#10315,18.);
#2243=CIRCLE('',#10316,18.);
#2244=CIRCLE('',#10318,18.);
#2245=CIRCLE('',#10319,18.);
#2246=CIRCLE('',#10321,18.);
#2247=CIRCLE('',#10322,18.);
#2248=CIRCLE('',#10324,18.);
#2249=CIRCLE('',#10325,18.);
#2250=CIRCLE('',#10327,18.);
#2251=CIRCLE('',#10328,18.);
#2252=CIRCLE('',#10330,18.);
#2253=CIRCLE('',#10331,18.);
#2254=CIRCLE('',#10333,18.);
#2255=CIRCLE('',#10334,18.);
#2256=CIRCLE('',#10336,18.);
#2257=CIRCLE('',#10337,18.);
#2258=CIRCLE('',#10339,18.);
#2259=CIRCLE('',#10340,18.);
#2260=CIRCLE('',#10342,18.);
#2261=CIRCLE('',#10343,18.);
#2262=CIRCLE('',#10345,18.);
#2263=CIRCLE('',#10346,18.);
#2264=CIRCLE('',#10348,18.);
#2265=CIRCLE('',#10349,18.);
#2266=CIRCLE('',#10351,18.);
#2267=CIRCLE('',#10352,18.);
#2268=CIRCLE('',#10354,18.);
#2269=CIRCLE('',#10355,18.);
#2270=CIRCLE('',#10357,18.);
#2271=CIRCLE('',#10358,18.);
#2272=CIRCLE('',#10360,18.);
#2273=CIRCLE('',#10361,18.);
#2274=CIRCLE('',#10363,18.);
#2275=CIRCLE('',#10364,18.);
#2276=CIRCLE('',#10366,18.);
#2277=CIRCLE('',#10367,18.);
#2278=CIRCLE('',#10369,18.);
#2279=CIRCLE('',#10370,18.);
#2280=CIRCLE('',#10372,18.);
#2281=CIRCLE('',#10373,18.);
#2282=CIRCLE('',#10375,18.);
#2283=CIRCLE('',#10376,18.);
#2284=CIRCLE('',#10378,18.);
#2285=CIRCLE('',#10379,18.);
#2286=CIRCLE('',#10381,18.);
#2287=CIRCLE('',#10382,18.);
#2288=CIRCLE('',#10384,18.);
#2289=CIRCLE('',#10385,18.);
#2290=CIRCLE('',#10387,18.);
#2291=CIRCLE('',#10388,18.);
#2292=CIRCLE('',#10470,25.);
#2293=CIRCLE('',#10471,25.);
#2294=CIRCLE('',#10473,24.);
#2295=CIRCLE('',#10475,24.);
#2296=CIRCLE('',#10476,20.);
#2297=CIRCLE('',#10478,10.75);
#2298=CIRCLE('',#10479,40.);
#2299=CIRCLE('',#10480,40.);
#2300=CIRCLE('',#10483,40.);
#2301=CIRCLE('',#10486,40.);
#2302=CIRCLE('',#10488,20.);
#2303=CIRCLE('',#10490,1.);
#2304=CIRCLE('',#10491,1.);
#2305=CIRCLE('',#10493,1.);
#2306=CIRCLE('',#10494,1.);
#2307=CIRCLE('',#10495,0.999999999999999);
#2308=CIRCLE('',#10496,1.);
#2309=CIRCLE('',#10498,1.);
#2310=CIRCLE('',#10499,1.);
#2311=CIRCLE('',#10501,10.7);
#2312=CIRCLE('',#10503,8.35);
#2313=CIRCLE('',#10504,8.35);
#2314=CIRCLE('',#10505,9.33888888888891);
#2315=CIRCLE('',#10506,8.35);
#2316=CIRCLE('',#10508,6.18146853146853);
#2317=CIRCLE('',#10510,2.35);
#2318=CIRCLE('',#10527,2.8);
#2319=CIRCLE('',#10530,17.85);
#2320=CIRCLE('',#10531,17.85);
#2321=CIRCLE('',#10532,17.85);
#2322=CIRCLE('',#10533,17.85);
#2323=CIRCLE('',#10535,20.);
#2324=CIRCLE('',#10536,15.);
#2325=CIRCLE('',#10538,20.);
#2326=CIRCLE('',#10539,20.);
#2327=CIRCLE('',#10541,19.5);
#2328=CIRCLE('',#10543,15.);
#2329=CIRCLE('',#10545,5.50000000000001);
#2330=CIRCLE('',#10546,3.);
#2331=CIRCLE('',#10548,17.85);
#2332=CIRCLE('',#10549,16.5);
#2333=CIRCLE('',#10551,16.5);
#2334=CIRCLE('',#10554,17.85);
#2335=CIRCLE('',#10557,3.);
#2336=CIRCLE('',#10559,5.);
#2337=CIRCLE('',#10560,5.);
#2338=CIRCLE('',#10561,5.);
#2339=CIRCLE('',#10562,5.);
#2340=CIRCLE('',#10565,3.);
#2341=CIRCLE('',#10570,3.);
#2342=CIRCLE('',#10573,2.8);
#2343=CIRCLE('',#10576,6.08697438789325);
#2344=CIRCLE('',#10582,17.1);
#2345=CIRCLE('',#10583,17.1);
#2346=CIRCLE('',#10585,9.);
#2347=CIRCLE('',#10586,9.);
#2348=CIRCLE('',#10590,3.50000000000001);
#2349=CIRCLE('',#10592,3.50000000000001);
#2350=CIRCLE('',#10594,3.);
#2351=CIRCLE('',#10595,3.);
#2352=CIRCLE('',#10596,3.);
#2353=CIRCLE('',#10617,3.);
#2354=CIRCLE('',#10618,3.);
#2355=CIRCLE('',#10619,3.);
#2356=CIRCLE('',#10621,2.5);
#2357=CIRCLE('',#10623,2.5);
#2358=CIRCLE('',#10628,4.50000000000001);
#2359=CIRCLE('',#10630,5.);
#2360=CIRCLE('',#10631,5.);
#2361=CIRCLE('',#10632,5.);
#2362=CIRCLE('',#10634,14.5);
#2363=CIRCLE('',#10636,15.);
#2364=CIRCLE('',#10637,15.);
#2365=CIRCLE('',#10638,15.);
#2366=CIRCLE('',#10640,12.5);
#2367=CIRCLE('',#10641,1.);
#2368=CIRCLE('',#10642,1.);
#2369=CIRCLE('',#10643,12.5);
#2370=CIRCLE('',#10644,1.);
#2371=CIRCLE('',#10645,1.);
#2372=CIRCLE('',#10647,12.5);
#2373=CIRCLE('',#10650,12.5);
#2374=CIRCLE('',#10653,1.);
#2375=CIRCLE('',#10654,1.);
#2376=CIRCLE('',#10655,1.);
#2377=CIRCLE('',#10656,1.);
#2378=CIRCLE('',#10658,2.8);
#2379=CIRCLE('',#10667,0.35);
#2380=CIRCLE('',#10668,0.35);
#2381=CIRCLE('',#10669,0.35);
#2382=CIRCLE('',#10670,0.35);
#2383=CIRCLE('',#10671,0.35);
#2384=CIRCLE('',#10672,0.35);
#2385=CIRCLE('',#10673,0.35);
#2386=CIRCLE('',#10674,0.35);
#2387=CIRCLE('',#10678,0.35);
#2388=CIRCLE('',#10679,0.35);
#2389=CIRCLE('',#10680,0.35);
#2390=CIRCLE('',#10681,0.35);
#2391=CIRCLE('',#10682,0.35);
#2392=CIRCLE('',#10683,0.35);
#2393=CIRCLE('',#10684,0.35);
#2394=CIRCLE('',#10685,0.35);
#2395=CIRCLE('',#10690,2.75);
#2396=CIRCLE('',#10701,1.65);
#2397=CIRCLE('',#10702,6.9);
#2398=CIRCLE('',#10706,11.1);
#2399=CIRCLE('',#10707,11.1);
#2400=CIRCLE('',#10709,11.1);
#2401=CIRCLE('',#10710,11.1);
#2402=CIRCLE('',#10712,11.1);
#2403=CIRCLE('',#10713,11.1);
#2404=CIRCLE('',#10714,11.1);
#2405=CIRCLE('',#10716,10.6);
#2406=CIRCLE('',#10717,9.69998799999997);
#2407=CIRCLE('',#10719,10.6);
#2408=CIRCLE('',#10720,9.70000000000007);
#2409=CIRCLE('',#10722,9.2);
#2410=CIRCLE('',#10723,9.2);
#2411=CIRCLE('',#10724,9.2);
#2412=CIRCLE('',#10730,0.8);
#2413=CIRCLE('',#10732,0.8);
#2414=CIRCLE('',#10733,1.865);
#2415=CIRCLE('',#10735,1.865);
#2416=CIRCLE('',#10736,1.865);
#2417=CIRCLE('',#10738,1.865);
#2418=CIRCLE('',#10739,1.865);
#2419=CIRCLE('',#10741,1.865);
#2420=CIRCLE('',#10742,1.865);
#2421=CIRCLE('',#10744,1.865);
#2422=CIRCLE('',#10745,1.865);
#2423=CIRCLE('',#10747,1.865);
#2424=CIRCLE('',#10748,1.865);
#2425=CIRCLE('',#10750,1.865);
#2426=CIRCLE('',#10751,1.865);
#2427=CIRCLE('',#10753,1.865);
#2428=CIRCLE('',#10754,1.865);
#2429=CIRCLE('',#10756,1.865);
#2430=CIRCLE('',#10757,1.865);
#2431=CIRCLE('',#10759,1.865);
#2432=CIRCLE('',#10760,1.865);
#2433=CIRCLE('',#10762,1.865);
#2434=CIRCLE('',#10769,9.1);
#2435=CIRCLE('',#10770,9.1);
#2436=CIRCLE('',#10772,3.5);
#2437=CIRCLE('',#10774,3.5);
#2438=CIRCLE('',#10776,2.125);
#2439=CIRCLE('',#10779,2.125);
#2440=CIRCLE('',#10784,5.);
#2441=CIRCLE('',#10785,3.);
#2442=CIRCLE('',#10787,5.);
#2443=CIRCLE('',#10789,4.5);
#2444=CIRCLE('',#10790,1.75);
#2445=CIRCLE('',#10792,1.75);
#2446=CIRCLE('',#10794,0.5);
#2447=CIRCLE('',#10796,3.);
#2448=CIRCLE('',#10798,2.4455);
#2449=CIRCLE('',#10809,2.);
#2450=CIRCLE('',#10811,2.);
#2451=CIRCLE('',#10816,9.15);
#2452=CIRCLE('',#10817,9.15);
#2453=CIRCLE('',#10818,9.15);
#2454=CIRCLE('',#10820,6.75);
#2455=CIRCLE('',#10822,8.15);
#2456=CIRCLE('',#10823,3.57071421427142);
#2457=CIRCLE('',#10825,6.75);
#2458=CIRCLE('',#10833,1.);
#2459=CIRCLE('',#10870,0.375000000000001);
#2460=CIRCLE('',#10871,10.2);
#2461=CIRCLE('',#10872,0.375000000000001);
#2462=CIRCLE('',#10877,8.925);
#2463=CIRCLE('',#10878,8.925);
#2464=CIRCLE('',#10883,9.15);
#2465=CIRCLE('',#10884,7.25);
#2466=CIRCLE('',#10886,9.15);
#2467=CIRCLE('',#10887,7.25);
#2468=CIRCLE('',#10906,3.);
#2469=CIRCLE('',#10907,3.);
#2470=CIRCLE('',#10909,3.75);
#2471=CIRCLE('',#10911,3.75);
#2472=CIRCLE('',#10914,3.);
#2473=CIRCLE('',#10915,2.4);
#2474=CIRCLE('',#10917,2.4);
#2475=CIRCLE('',#10920,3.);
#2476=CIRCLE('',#10925,17.5);
#2477=CIRCLE('',#10926,17.5);
#2478=CIRCLE('',#10928,17.5);
#2479=CIRCLE('',#10929,17.5);
#2480=CIRCLE('',#10931,17.5);
#2481=CIRCLE('',#10932,17.5);
#2482=CIRCLE('',#10934,17.5);
#2483=CIRCLE('',#10935,17.5);
#2484=CIRCLE('',#10936,17.5);
#2485=CIRCLE('',#10938,17.5);
#2486=CIRCLE('',#10939,17.5);
#2487=CIRCLE('',#10941,17.5);
#2488=CIRCLE('',#10942,17.5);
#2489=CIRCLE('',#10944,17.5);
#2490=CIRCLE('',#10945,17.5);
#2491=CIRCLE('',#10947,17.5);
#2492=CIRCLE('',#10948,17.5);
#2493=CIRCLE('',#10950,17.5);
#2494=CIRCLE('',#10951,17.5);
#2495=CIRCLE('',#10953,4.98804347826086);
#2496=CIRCLE('',#10954,4.98804347826086);
#2497=CIRCLE('',#10955,4.98804347826086);
#2498=CIRCLE('',#10956,4.98804347826086);
#2499=CIRCLE('',#10957,4.98804347826086);
#2500=CIRCLE('',#10958,4.98804347826086);
#2501=CIRCLE('',#10959,4.98804347826086);
#2502=CIRCLE('',#10960,4.98804347826086);
#2503=CIRCLE('',#10961,17.5);
#2504=CIRCLE('',#10962,4.98804347826086);
#2505=CIRCLE('',#10963,4.98804347826087);
#2506=CIRCLE('',#10964,15.);
#2507=CIRCLE('',#10966,14.);
#2508=CIRCLE('',#10967,14.);
#2509=CIRCLE('',#10969,14.);
#2510=CIRCLE('',#10970,14.);
#2511=CIRCLE('',#10972,17.5);
#2512=CIRCLE('',#10974,12.35);
#2513=CIRCLE('',#10975,11.35);
#2514=CIRCLE('',#10977,13.);
#2515=CIRCLE('',#10978,13.);
#2516=CIRCLE('',#10980,13.);
#2517=CIRCLE('',#10982,16.);
#2518=CIRCLE('',#10984,16.);
#2519=CIRCLE('',#10985,16.);
#2520=CIRCLE('',#10988,11.35);
#2521=CIRCLE('',#10996,15.);
#2522=CIRCLE('',#10999,15.5);
#2523=CIRCLE('',#11001,15.5);
#2524=CIRCLE('',#11004,4.48804347826086);
#2525=CIRCLE('',#11006,4.48804347826086);
#2526=CIRCLE('',#11008,4.48804347826086);
#2527=CIRCLE('',#11010,4.48804347826086);
#2528=CIRCLE('',#11012,4.48804347826086);
#2529=CIRCLE('',#11014,4.48804347826086);
#2530=CIRCLE('',#11016,4.48804347826086);
#2531=CIRCLE('',#11018,4.48804347826086);
#2532=CIRCLE('',#11020,4.48804347826086);
#2533=CIRCLE('',#11022,4.48804347826087);
#2534=CIRCLE('',#11061,13.8985);
#2535=CIRCLE('',#11062,4.5);
#2536=CIRCLE('',#11064,14.5);
#2537=CIRCLE('',#11072,4.5);
#2538=CIRCLE('',#11073,4.5);
#2539=CIRCLE('',#11075,15.);
#2540=CIRCLE('',#11076,15.);
#2541=CIRCLE('',#11077,15.);
#2542=CIRCLE('',#11079,6.50000000000001);
#2543=CIRCLE('',#11100,0.5);
#2544=CIRCLE('',#11103,0.6);
#2545=CIRCLE('',#11104,0.6);
#2546=CIRCLE('',#11105,0.6);
#2547=CIRCLE('',#11106,0.6);
#2548=CIRCLE('',#11107,0.6);
#2549=CIRCLE('',#11108,0.6);
#2550=CIRCLE('',#11109,0.6);
#2551=CIRCLE('',#11110,0.6);
#2552=CIRCLE('',#11115,19.);
#2553=CIRCLE('',#11116,16.1);
#2554=CIRCLE('',#11118,19.);
#2555=CIRCLE('',#11120,45.);
#2556=CIRCLE('',#11121,17.);
#2557=CIRCLE('',#11123,16.);
#2558=CIRCLE('',#11125,13.1);
#2559=CIRCLE('',#11127,13.1);
#2560=CIRCLE('',#11129,15.1);
#2561=CIRCLE('',#11131,15.1);
#2562=CIRCLE('',#11132,15.1);
#2563=CIRCLE('',#11134,14.1);
#2564=CIRCLE('',#11135,14.1);
#2565=CIRCLE('',#11137,14.1);
#2566=CIRCLE('',#11138,14.1);
#2567=CIRCLE('',#11140,13.1);
#2568=CIRCLE('',#11141,13.1);
#2569=CIRCLE('',#11143,13.1);
#2570=CIRCLE('',#11145,16.1);
#2571=CIRCLE('',#11149,1.75);
#2572=CIRCLE('',#11161,11.);
#2573=CIRCLE('',#11163,15.75);
#2574=CIRCLE('',#11165,15.75);
#2575=CIRCLE('',#11166,15.75);
#2576=CIRCLE('',#11168,15.25);
#2577=CIRCLE('',#11169,13.5);
#2578=CIRCLE('',#11171,13.5);
#2579=CIRCLE('',#11172,13.5);
#2580=CIRCLE('',#11175,12.3985);
#2581=CIRCLE('',#11177,9.);
#2582=CIRCLE('',#11179,9.);
#2583=CIRCLE('',#11181,10.);
#2584=CIRCLE('',#11185,1.31);
#2585=CIRCLE('',#11186,11.735);
#2586=CIRCLE('',#11189,6.50555349946514);
#2587=CIRCLE('',#11190,6.50555349946514);
#2588=CIRCLE('',#11191,6.50555349946514);
#2589=CIRCLE('',#11192,6.50555349946514);
#2590=CIRCLE('',#11193,6.50555349946514);
#2591=CIRCLE('',#11194,6.50555349946514);
#2592=CIRCLE('',#11195,3.5);
#2593=CIRCLE('',#11197,6.50555349946514);
#2594=CIRCLE('',#11198,6.50555349946514);
#2595=CIRCLE('',#11199,6.50555349946514);
#2596=CIRCLE('',#11200,6.50555349946514);
#2597=CIRCLE('',#11201,6.50555349946514);
#2598=CIRCLE('',#11202,6.50555349946514);
#2599=CIRCLE('',#11203,3.5);
#2600=LINE('',#13920,#3350);
#2601=LINE('',#13924,#3351);
#2602=LINE('',#13929,#3352);
#2603=LINE('',#13933,#3353);
#2604=LINE('',#13938,#3354);
#2605=LINE('',#13942,#3355);
#2606=LINE('',#13947,#3356);
#2607=LINE('',#13951,#3357);
#2608=LINE('',#13956,#3358);
#2609=LINE('',#13960,#3359);
#2610=LINE('',#13965,#3360);
#2611=LINE('',#13969,#3361);
#2612=LINE('',#13974,#3362);
#2613=LINE('',#13978,#3363);
#2614=LINE('',#13983,#3364);
#2615=LINE('',#13987,#3365);
#2616=LINE('',#13992,#3366);
#2617=LINE('',#13996,#3367);
#2618=LINE('',#14001,#3368);
#2619=LINE('',#14005,#3369);
#2620=LINE('',#14010,#3370);
#2621=LINE('',#14014,#3371);
#2622=LINE('',#14019,#3372);
#2623=LINE('',#14023,#3373);
#2624=LINE('',#14028,#3374);
#2625=LINE('',#14032,#3375);
#2626=LINE('',#14037,#3376);
#2627=LINE('',#14041,#3377);
#2628=LINE('',#14046,#3378);
#2629=LINE('',#14050,#3379);
#2630=LINE('',#14055,#3380);
#2631=LINE('',#14059,#3381);
#2632=LINE('',#14064,#3382);
#2633=LINE('',#14068,#3383);
#2634=LINE('',#14073,#3384);
#2635=LINE('',#14077,#3385);
#2636=LINE('',#14082,#3386);
#2637=LINE('',#14086,#3387);
#2638=LINE('',#14091,#3388);
#2639=LINE('',#14095,#3389);
#2640=LINE('',#14100,#3390);
#2641=LINE('',#14104,#3391);
#2642=LINE('',#14109,#3392);
#2643=LINE('',#14113,#3393);
#2644=LINE('',#14118,#3394);
#2645=LINE('',#14122,#3395);
#2646=LINE('',#14127,#3396);
#2647=LINE('',#14131,#3397);
#2648=LINE('',#14136,#3398);
#2649=LINE('',#14140,#3399);
#2650=LINE('',#14145,#3400);
#2651=LINE('',#14149,#3401);
#2652=LINE('',#14154,#3402);
#2653=LINE('',#14158,#3403);
#2654=LINE('',#14163,#3404);
#2655=LINE('',#14167,#3405);
#2656=LINE('',#14172,#3406);
#2657=LINE('',#14176,#3407);
#2658=LINE('',#14181,#3408);
#2659=LINE('',#14185,#3409);
#2660=LINE('',#14190,#3410);
#2661=LINE('',#14194,#3411);
#2662=LINE('',#14199,#3412);
#2663=LINE('',#14203,#3413);
#2664=LINE('',#14208,#3414);
#2665=LINE('',#14212,#3415);
#2666=LINE('',#14217,#3416);
#2667=LINE('',#14221,#3417);
#2668=LINE('',#14226,#3418);
#2669=LINE('',#14230,#3419);
#2670=LINE('',#14235,#3420);
#2671=LINE('',#14239,#3421);
#2672=LINE('',#14244,#3422);
#2673=LINE('',#14248,#3423);
#2674=LINE('',#14253,#3424);
#2675=LINE('',#14257,#3425);
#2676=LINE('',#14262,#3426);
#2677=LINE('',#14266,#3427);
#2678=LINE('',#14271,#3428);
#2679=LINE('',#14275,#3429);
#2680=LINE('',#14279,#3430);
#2681=LINE('',#14281,#3431);
#2682=LINE('',#14282,#3432);
#2683=LINE('',#14284,#3433);
#2684=LINE('',#14285,#3434);
#2685=LINE('',#14288,#3435);
#2686=LINE('',#14290,#3436);
#2687=LINE('',#14291,#3437);
#2688=LINE('',#14293,#3438);
#2689=LINE('',#14294,#3439);
#2690=LINE('',#14297,#3440);
#2691=LINE('',#14299,#3441);
#2692=LINE('',#14300,#3442);
#2693=LINE('',#14302,#3443);
#2694=LINE('',#14303,#3444);
#2695=LINE('',#14306,#3445);
#2696=LINE('',#14308,#3446);
#2697=LINE('',#14309,#3447);
#2698=LINE('',#14311,#3448);
#2699=LINE('',#14312,#3449);
#2700=LINE('',#14315,#3450);
#2701=LINE('',#14317,#3451);
#2702=LINE('',#14318,#3452);
#2703=LINE('',#14320,#3453);
#2704=LINE('',#14321,#3454);
#2705=LINE('',#14324,#3455);
#2706=LINE('',#14326,#3456);
#2707=LINE('',#14327,#3457);
#2708=LINE('',#14329,#3458);
#2709=LINE('',#14330,#3459);
#2710=LINE('',#14333,#3460);
#2711=LINE('',#14335,#3461);
#2712=LINE('',#14336,#3462);
#2713=LINE('',#14338,#3463);
#2714=LINE('',#14339,#3464);
#2715=LINE('',#14342,#3465);
#2716=LINE('',#14344,#3466);
#2717=LINE('',#14345,#3467);
#2718=LINE('',#14347,#3468);
#2719=LINE('',#14348,#3469);
#2720=LINE('',#14351,#3470);
#2721=LINE('',#14353,#3471);
#2722=LINE('',#14354,#3472);
#2723=LINE('',#14356,#3473);
#2724=LINE('',#14357,#3474);
#2725=LINE('',#14360,#3475);
#2726=LINE('',#14362,#3476);
#2727=LINE('',#14363,#3477);
#2728=LINE('',#14365,#3478);
#2729=LINE('',#14366,#3479);
#2730=LINE('',#14369,#3480);
#2731=LINE('',#14371,#3481);
#2732=LINE('',#14372,#3482);
#2733=LINE('',#14374,#3483);
#2734=LINE('',#14375,#3484);
#2735=LINE('',#14378,#3485);
#2736=LINE('',#14380,#3486);
#2737=LINE('',#14381,#3487);
#2738=LINE('',#14383,#3488);
#2739=LINE('',#14384,#3489);
#2740=LINE('',#14387,#3490);
#2741=LINE('',#14389,#3491);
#2742=LINE('',#14390,#3492);
#2743=LINE('',#14392,#3493);
#2744=LINE('',#14393,#3494);
#2745=LINE('',#14396,#3495);
#2746=LINE('',#14398,#3496);
#2747=LINE('',#14399,#3497);
#2748=LINE('',#14401,#3498);
#2749=LINE('',#14402,#3499);
#2750=LINE('',#14405,#3500);
#2751=LINE('',#14407,#3501);
#2752=LINE('',#14408,#3502);
#2753=LINE('',#14410,#3503);
#2754=LINE('',#14411,#3504);
#2755=LINE('',#14414,#3505);
#2756=LINE('',#14416,#3506);
#2757=LINE('',#14417,#3507);
#2758=LINE('',#14419,#3508);
#2759=LINE('',#14420,#3509);
#2760=LINE('',#14423,#3510);
#2761=LINE('',#14425,#3511);
#2762=LINE('',#14426,#3512);
#2763=LINE('',#14428,#3513);
#2764=LINE('',#14429,#3514);
#2765=LINE('',#14432,#3515);
#2766=LINE('',#14434,#3516);
#2767=LINE('',#14435,#3517);
#2768=LINE('',#14437,#3518);
#2769=LINE('',#14438,#3519);
#2770=LINE('',#14441,#3520);
#2771=LINE('',#14443,#3521);
#2772=LINE('',#14444,#3522);
#2773=LINE('',#14446,#3523);
#2774=LINE('',#14447,#3524);
#2775=LINE('',#14450,#3525);
#2776=LINE('',#14452,#3526);
#2777=LINE('',#14453,#3527);
#2778=LINE('',#14455,#3528);
#2779=LINE('',#14456,#3529);
#2780=LINE('',#14459,#3530);
#2781=LINE('',#14461,#3531);
#2782=LINE('',#14462,#3532);
#2783=LINE('',#14464,#3533);
#2784=LINE('',#14465,#3534);
#2785=LINE('',#14468,#3535);
#2786=LINE('',#14470,#3536);
#2787=LINE('',#14471,#3537);
#2788=LINE('',#14473,#3538);
#2789=LINE('',#14474,#3539);
#2790=LINE('',#14477,#3540);
#2791=LINE('',#14479,#3541);
#2792=LINE('',#14480,#3542);
#2793=LINE('',#14482,#3543);
#2794=LINE('',#14483,#3544);
#2795=LINE('',#14486,#3545);
#2796=LINE('',#14488,#3546);
#2797=LINE('',#14489,#3547);
#2798=LINE('',#14491,#3548);
#2799=LINE('',#14492,#3549);
#2800=LINE('',#14495,#3550);
#2801=LINE('',#14497,#3551);
#2802=LINE('',#14498,#3552);
#2803=LINE('',#14500,#3553);
#2804=LINE('',#14501,#3554);
#2805=LINE('',#14504,#3555);
#2806=LINE('',#14506,#3556);
#2807=LINE('',#14507,#3557);
#2808=LINE('',#14509,#3558);
#2809=LINE('',#14510,#3559);
#2810=LINE('',#14513,#3560);
#2811=LINE('',#14515,#3561);
#2812=LINE('',#14516,#3562);
#2813=LINE('',#14518,#3563);
#2814=LINE('',#14519,#3564);
#2815=LINE('',#14522,#3565);
#2816=LINE('',#14524,#3566);
#2817=LINE('',#14525,#3567);
#2818=LINE('',#14527,#3568);
#2819=LINE('',#14528,#3569);
#2820=LINE('',#14531,#3570);
#2821=LINE('',#14533,#3571);
#2822=LINE('',#14534,#3572);
#2823=LINE('',#14536,#3573);
#2824=LINE('',#14537,#3574);
#2825=LINE('',#14540,#3575);
#2826=LINE('',#14542,#3576);
#2827=LINE('',#14543,#3577);
#2828=LINE('',#14545,#3578);
#2829=LINE('',#14546,#3579);
#2830=LINE('',#14549,#3580);
#2831=LINE('',#14551,#3581);
#2832=LINE('',#14552,#3582);
#2833=LINE('',#14554,#3583);
#2834=LINE('',#14555,#3584);
#2835=LINE('',#14558,#3585);
#2836=LINE('',#14560,#3586);
#2837=LINE('',#14561,#3587);
#2838=LINE('',#14563,#3588);
#2839=LINE('',#14564,#3589);
#2840=LINE('',#14567,#3590);
#2841=LINE('',#14569,#3591);
#2842=LINE('',#14570,#3592);
#2843=LINE('',#14572,#3593);
#2844=LINE('',#14573,#3594);
#2845=LINE('',#14576,#3595);
#2846=LINE('',#14578,#3596);
#2847=LINE('',#14579,#3597);
#2848=LINE('',#14581,#3598);
#2849=LINE('',#14582,#3599);
#2850=LINE('',#14585,#3600);
#2851=LINE('',#14587,#3601);
#2852=LINE('',#14588,#3602);
#2853=LINE('',#14590,#3603);
#2854=LINE('',#14591,#3604);
#2855=LINE('',#14594,#3605);
#2856=LINE('',#14596,#3606);
#2857=LINE('',#14597,#3607);
#2858=LINE('',#14599,#3608);
#2859=LINE('',#14600,#3609);
#2860=LINE('',#14603,#3610);
#2861=LINE('',#14605,#3611);
#2862=LINE('',#14606,#3612);
#2863=LINE('',#14608,#3613);
#2864=LINE('',#14609,#3614);
#2865=LINE('',#14612,#3615);
#2866=LINE('',#14614,#3616);
#2867=LINE('',#14615,#3617);
#2868=LINE('',#14617,#3618);
#2869=LINE('',#14618,#3619);
#2870=LINE('',#14621,#3620);
#2871=LINE('',#14623,#3621);
#2872=LINE('',#14624,#3622);
#2873=LINE('',#14626,#3623);
#2874=LINE('',#14627,#3624);
#2875=LINE('',#14630,#3625);
#2876=LINE('',#14632,#3626);
#2877=LINE('',#14633,#3627);
#2878=LINE('',#14635,#3628);
#2879=LINE('',#14636,#3629);
#2880=LINE('',#15043,#3630);
#2881=LINE('',#16673,#3631);
#2882=LINE('',#16992,#3632);
#2883=LINE('',#17628,#3633);
#2884=LINE('',#17633,#3634);
#2885=LINE('',#17637,#3635);
#2886=LINE('',#17639,#3636);
#2887=LINE('',#17641,#3637);
#2888=LINE('',#17642,#3638);
#2889=LINE('',#17645,#3639);
#2890=LINE('',#17647,#3640);
#2891=LINE('',#17648,#3641);
#2892=LINE('',#17651,#3642);
#2893=LINE('',#17652,#3643);
#2894=LINE('',#17655,#3644);
#2895=LINE('',#17656,#3645);
#2896=LINE('',#17658,#3646);
#2897=LINE('',#17669,#3647);
#2898=LINE('',#17671,#3648);
#2899=LINE('',#17672,#3649);
#2900=LINE('',#17679,#3650);
#2901=LINE('',#17680,#3651);
#2902=LINE('',#17687,#3652);
#2903=LINE('',#17688,#3653);
#2904=LINE('',#17695,#3654);
#2905=LINE('',#17696,#3655);
#2906=LINE('',#17703,#3656);
#2907=LINE('',#17705,#3657);
#2908=LINE('',#17715,#3658);
#2909=LINE('',#17716,#3659);
#2910=LINE('',#17723,#3660);
#2911=LINE('',#17724,#3661);
#2912=LINE('',#17731,#3662);
#2913=LINE('',#17736,#3663);
#2914=LINE('',#17738,#3664);
#2915=LINE('',#17740,#3665);
#2916=LINE('',#17745,#3666);
#2917=LINE('',#17756,#3667);
#2918=LINE('',#17764,#3668);
#2919=LINE('',#17778,#3669);
#2920=LINE('',#17784,#3670);
#2921=LINE('',#17788,#3671);
#2922=LINE('',#17793,#3672);
#2923=LINE('',#17795,#3673);
#2924=LINE('',#17797,#3674);
#2925=LINE('',#17802,#3675);
#2926=LINE('',#17806,#3676);
#2927=LINE('',#17807,#3677);
#2928=LINE('',#17811,#3678);
#2929=LINE('',#17813,#3679);
#2930=LINE('',#17819,#3680);
#2931=LINE('',#17823,#3681);
#2932=LINE('',#17827,#3682);
#2933=LINE('',#17831,#3683);
#2934=LINE('',#17833,#3684);
#2935=LINE('',#17838,#3685);
#2936=LINE('',#17842,#3686);
#2937=LINE('',#17849,#3687);
#2938=LINE('',#17852,#3688);
#2939=LINE('',#17855,#3689);
#2940=LINE('',#17857,#3690);
#2941=LINE('',#17858,#3691);
#2942=LINE('',#17861,#3692);
#2943=LINE('',#17863,#3693);
#2944=LINE('',#17864,#3694);
#2945=LINE('',#17867,#3695);
#2946=LINE('',#17869,#3696);
#2947=LINE('',#17871,#3697);
#2948=LINE('',#17873,#3698);
#2949=LINE('',#17875,#3699);
#2950=LINE('',#17877,#3700);
#2951=LINE('',#17879,#3701);
#2952=LINE('',#17880,#3702);
#2953=LINE('',#17882,#3703);
#2954=LINE('',#17884,#3704);
#2955=LINE('',#17886,#3705);
#2956=LINE('',#17888,#3706);
#2957=LINE('',#17890,#3707);
#2958=LINE('',#17892,#3708);
#2959=LINE('',#17894,#3709);
#2960=LINE('',#17895,#3710);
#2961=LINE('',#17900,#3711);
#2962=LINE('',#17902,#3712);
#2963=LINE('',#17904,#3713);
#2964=LINE('',#17906,#3714);
#2965=LINE('',#17908,#3715);
#2966=LINE('',#17910,#3716);
#2967=LINE('',#17912,#3717);
#2968=LINE('',#17913,#3718);
#2969=LINE('',#17915,#3719);
#2970=LINE('',#17917,#3720);
#2971=LINE('',#17919,#3721);
#2972=LINE('',#17921,#3722);
#2973=LINE('',#17923,#3723);
#2974=LINE('',#17925,#3724);
#2975=LINE('',#17927,#3725);
#2976=LINE('',#17928,#3726);
#2977=LINE('',#17936,#3727);
#2978=LINE('',#17940,#3728);
#2979=LINE('',#17942,#3729);
#2980=LINE('',#17944,#3730);
#2981=LINE('',#17946,#3731);
#2982=LINE('',#17948,#3732);
#2983=LINE('',#17950,#3733);
#2984=LINE('',#17952,#3734);
#2985=LINE('',#17955,#3735);
#2986=LINE('',#17957,#3736);
#2987=LINE('',#17959,#3737);
#2988=LINE('',#17961,#3738);
#2989=LINE('',#17963,#3739);
#2990=LINE('',#17965,#3740);
#2991=LINE('',#17967,#3741);
#2992=LINE('',#17970,#3742);
#2993=LINE('',#17972,#3743);
#2994=LINE('',#17980,#3744);
#2995=LINE('',#17989,#3745);
#2996=LINE('',#17991,#3746);
#2997=LINE('',#18001,#3747);
#2998=LINE('',#18050,#3748);
#2999=LINE('',#18060,#3749);
#3000=LINE('',#18068,#3750);
#3001=LINE('',#18074,#3751);
#3002=LINE('',#18075,#3752);
#3003=LINE('',#18078,#3753);
#3004=LINE('',#18080,#3754);
#3005=LINE('',#18081,#3755);
#3006=LINE('',#18084,#3756);
#3007=LINE('',#18087,#3757);
#3008=LINE('',#18090,#3758);
#3009=LINE('',#18092,#3759);
#3010=LINE('',#18093,#3760);
#3011=LINE('',#18102,#3761);
#3012=LINE('',#18105,#3762);
#3013=LINE('',#18107,#3763);
#3014=LINE('',#21098,#3764);
#3015=LINE('',#21119,#3765);
#3016=LINE('',#21138,#3766);
#3017=LINE('',#21160,#3767);
#3018=LINE('',#21210,#3768);
#3019=LINE('',#21242,#3769);
#3020=LINE('',#21276,#3770);
#3021=LINE('',#21308,#3771);
#3022=LINE('',#21342,#3772);
#3023=LINE('',#21374,#3773);
#3024=LINE('',#21408,#3774);
#3025=LINE('',#21440,#3775);
#3026=LINE('',#21474,#3776);
#3027=LINE('',#21506,#3777);
#3028=LINE('',#21540,#3778);
#3029=LINE('',#21572,#3779);
#3030=LINE('',#21606,#3780);
#3031=LINE('',#21638,#3781);
#3032=LINE('',#21672,#3782);
#3033=LINE('',#21704,#3783);
#3034=LINE('',#21738,#3784);
#3035=LINE('',#21770,#3785);
#3036=LINE('',#21775,#3786);
#3037=LINE('',#21799,#3787);
#3038=LINE('',#21866,#3788);
#3039=LINE('',#21892,#3789);
#3040=LINE('',#21974,#3790);
#3041=LINE('',#21998,#3791);
#3042=LINE('',#22022,#3792);
#3043=LINE('',#22146,#3793);
#3044=LINE('',#22148,#3794);
#3045=LINE('',#22189,#3795);
#3046=LINE('',#22208,#3796);
#3047=LINE('',#23768,#3797);
#3048=LINE('',#23770,#3798);
#3049=LINE('',#23772,#3799);
#3050=LINE('',#23774,#3800);
#3051=LINE('',#23780,#3801);
#3052=LINE('',#23804,#3802);
#3053=LINE('',#23874,#3803);
#3054=LINE('',#23879,#3804);
#3055=LINE('',#23882,#3805);
#3056=LINE('',#23891,#3806);
#3057=LINE('',#23905,#3807);
#3058=LINE('',#23909,#3808);
#3059=LINE('',#23914,#3809);
#3060=LINE('',#23916,#3810);
#3061=LINE('',#23918,#3811);
#3062=LINE('',#23920,#3812);
#3063=LINE('',#23922,#3813);
#3064=LINE('',#23923,#3814);
#3065=LINE('',#23927,#3815);
#3066=LINE('',#23928,#3816);
#3067=LINE('',#23929,#3817);
#3068=LINE('',#23932,#3818);
#3069=LINE('',#23933,#3819);
#3070=LINE('',#23936,#3820);
#3071=LINE('',#23937,#3821);
#3072=LINE('',#23940,#3822);
#3073=LINE('',#23941,#3823);
#3074=LINE('',#23944,#3824);
#3075=LINE('',#23945,#3825);
#3076=LINE('',#23947,#3826);
#3077=LINE('',#23954,#3827);
#3078=LINE('',#23958,#3828);
#3079=LINE('',#27735,#3829);
#3080=LINE('',#27747,#3830);
#3081=LINE('',#27752,#3831);
#3082=LINE('',#27754,#3832);
#3083=LINE('',#27756,#3833);
#3084=LINE('',#27757,#3834);
#3085=LINE('',#27760,#3835);
#3086=LINE('',#27762,#3836);
#3087=LINE('',#27763,#3837);
#3088=LINE('',#27766,#3838);
#3089=LINE('',#27767,#3839);
#3090=LINE('',#27770,#3840);
#3091=LINE('',#27771,#3841);
#3092=LINE('',#27773,#3842);
#3093=LINE('',#27782,#3843);
#3094=LINE('',#27784,#3844);
#3095=LINE('',#27786,#3845);
#3096=LINE('',#27787,#3846);
#3097=LINE('',#27790,#3847);
#3098=LINE('',#27792,#3848);
#3099=LINE('',#27794,#3849);
#3100=LINE('',#27796,#3850);
#3101=LINE('',#27798,#3851);
#3102=LINE('',#27800,#3852);
#3103=LINE('',#27802,#3853);
#3104=LINE('',#27804,#3854);
#3105=LINE('',#27806,#3855);
#3106=LINE('',#27808,#3856);
#3107=LINE('',#27810,#3857);
#3108=LINE('',#27811,#3858);
#3109=LINE('',#27815,#3859);
#3110=LINE('',#27816,#3860);
#3111=LINE('',#27817,#3861);
#3112=LINE('',#27820,#3862);
#3113=LINE('',#27821,#3863);
#3114=LINE('',#27824,#3864);
#3115=LINE('',#27825,#3865);
#3116=LINE('',#27827,#3866);
#3117=LINE('',#27831,#3867);
#3118=LINE('',#27833,#3868);
#3119=LINE('',#27835,#3869);
#3120=LINE('',#27837,#3870);
#3121=LINE('',#27839,#3871);
#3122=LINE('',#27841,#3872);
#3123=LINE('',#27843,#3873);
#3124=LINE('',#27845,#3874);
#3125=LINE('',#27847,#3875);
#3126=LINE('',#27849,#3876);
#3127=LINE('',#27851,#3877);
#3128=LINE('',#27852,#3878);
#3129=LINE('',#27855,#3879);
#3130=LINE('',#27857,#3880);
#3131=LINE('',#27858,#3881);
#3132=LINE('',#27861,#3882);
#3133=LINE('',#27862,#3883);
#3134=LINE('',#27865,#3884);
#3135=LINE('',#27866,#3885);
#3136=LINE('',#27869,#3886);
#3137=LINE('',#27870,#3887);
#3138=LINE('',#27873,#3888);
#3139=LINE('',#27874,#3889);
#3140=LINE('',#27877,#3890);
#3141=LINE('',#27878,#3891);
#3142=LINE('',#27881,#3892);
#3143=LINE('',#27882,#3893);
#3144=LINE('',#27885,#3894);
#3145=LINE('',#27886,#3895);
#3146=LINE('',#27889,#3896);
#3147=LINE('',#27890,#3897);
#3148=LINE('',#27893,#3898);
#3149=LINE('',#27894,#3899);
#3150=LINE('',#27897,#3900);
#3151=LINE('',#27898,#3901);
#3152=LINE('',#27900,#3902);
#3153=LINE('',#27904,#3903);
#3154=LINE('',#27906,#3904);
#3155=LINE('',#27907,#3905);
#3156=LINE('',#27910,#3906);
#3157=LINE('',#27911,#3907);
#3158=LINE('',#27914,#3908);
#3159=LINE('',#27915,#3909);
#3160=LINE('',#27918,#3910);
#3161=LINE('',#27919,#3911);
#3162=LINE('',#27922,#3912);
#3163=LINE('',#27923,#3913);
#3164=LINE('',#27926,#3914);
#3165=LINE('',#27927,#3915);
#3166=LINE('',#27930,#3916);
#3167=LINE('',#27931,#3917);
#3168=LINE('',#27934,#3918);
#3169=LINE('',#27935,#3919);
#3170=LINE('',#27938,#3920);
#3171=LINE('',#27939,#3921);
#3172=LINE('',#27942,#3922);
#3173=LINE('',#27943,#3923);
#3174=LINE('',#27946,#3924);
#3175=LINE('',#27947,#3925);
#3176=LINE('',#27949,#3926);
#3177=LINE('',#27965,#3927);
#3178=LINE('',#27981,#3928);
#3179=LINE('',#27983,#3929);
#3180=LINE('',#28003,#3930);
#3181=LINE('',#28010,#3931);
#3182=LINE('',#28020,#3932);
#3183=LINE('',#28027,#3933);
#3184=LINE('',#28044,#3934);
#3185=LINE('',#28062,#3935);
#3186=LINE('',#28072,#3936);
#3187=LINE('',#28092,#3937);
#3188=LINE('',#28111,#3938);
#3189=LINE('',#28131,#3939);
#3190=LINE('',#28150,#3940);
#3191=LINE('',#28170,#3941);
#3192=LINE('',#28202,#3942);
#3193=LINE('',#28220,#3943);
#3194=LINE('',#28230,#3944);
#3195=LINE('',#28250,#3945);
#3196=LINE('',#28269,#3946);
#3197=LINE('',#28289,#3947);
#3198=LINE('',#28308,#3948);
#3199=LINE('',#28328,#3949);
#3200=LINE('',#28347,#3950);
#3201=LINE('',#28367,#3951);
#3202=LINE('',#28403,#3952);
#3203=LINE('',#28409,#3953);
#3204=LINE('',#28414,#3954);
#3205=LINE('',#28431,#3955);
#3206=LINE('',#28457,#3956);
#3207=LINE('',#28460,#3957);
#3208=LINE('',#28658,#3958);
#3209=LINE('',#29066,#3959);
#3210=LINE('',#29260,#3960);
#3211=LINE('',#29453,#3961);
#3212=LINE('',#29455,#3962);
#3213=LINE('',#29457,#3963);
#3214=LINE('',#29459,#3964);
#3215=LINE('',#29461,#3965);
#3216=LINE('',#29465,#3966);
#3217=LINE('',#29467,#3967);
#3218=LINE('',#29473,#3968);
#3219=LINE('',#29479,#3969);
#3220=LINE('',#29483,#3970);
#3221=LINE('',#29505,#3971);
#3222=LINE('',#29509,#3972);
#3223=LINE('',#29595,#3973);
#3224=LINE('',#29599,#3974);
#3225=LINE('',#29621,#3975);
#3226=LINE('',#29625,#3976);
#3227=LINE('',#29714,#3977);
#3228=LINE('',#29718,#3978);
#3229=LINE('',#29823,#3979);
#3230=LINE('',#29826,#3980);
#3231=LINE('',#29830,#3981);
#3232=LINE('',#29834,#3982);
#3233=LINE('',#29920,#3983);
#3234=LINE('',#29924,#3984);
#3235=LINE('',#29946,#3985);
#3236=LINE('',#29950,#3986);
#3237=LINE('',#30039,#3987);
#3238=LINE('',#30043,#3988);
#3239=LINE('',#31169,#3989);
#3240=LINE('',#31171,#3990);
#3241=LINE('',#31173,#3991);
#3242=LINE('',#31175,#3992);
#3243=LINE('',#31177,#3993);
#3244=LINE('',#31179,#3994);
#3245=LINE('',#31181,#3995);
#3246=LINE('',#31183,#3996);
#3247=LINE('',#31185,#3997);
#3248=LINE('',#31187,#3998);
#3249=LINE('',#31189,#3999);
#3250=LINE('',#31191,#4000);
#3251=LINE('',#31193,#4001);
#3252=LINE('',#31195,#4002);
#3253=LINE('',#31197,#4003);
#3254=LINE('',#31199,#4004);
#3255=LINE('',#31201,#4005);
#3256=LINE('',#31203,#4006);
#3257=LINE('',#31205,#4007);
#3258=LINE('',#31207,#4008);
#3259=LINE('',#31209,#4009);
#3260=LINE('',#31211,#4010);
#3261=LINE('',#31213,#4011);
#3262=LINE('',#31214,#4012);
#3263=LINE('',#31218,#4013);
#3264=LINE('',#31219,#4014);
#3265=LINE('',#31220,#4015);
#3266=LINE('',#31224,#4016);
#3267=LINE('',#31225,#4017);
#3268=LINE('',#31226,#4018);
#3269=LINE('',#31230,#4019);
#3270=LINE('',#31231,#4020);
#3271=LINE('',#31232,#4021);
#3272=LINE('',#31235,#4022);
#3273=LINE('',#31237,#4023);
#3274=LINE('',#31238,#4024);
#3275=LINE('',#31241,#4025);
#3276=LINE('',#31242,#4026);
#3277=LINE('',#31246,#4027);
#3278=LINE('',#31247,#4028);
#3279=LINE('',#31248,#4029);
#3280=LINE('',#31254,#4030);
#3281=LINE('',#31261,#4031);
#3282=LINE('',#31266,#4032);
#3283=LINE('',#31268,#4033);
#3284=LINE('',#31269,#4034);
#3285=LINE('',#31271,#4035);
#3286=LINE('',#31273,#4036);
#3287=LINE('',#31274,#4037);
#3288=LINE('',#31276,#4038);
#3289=LINE('',#31278,#4039);
#3290=LINE('',#31279,#4040);
#3291=LINE('',#31281,#4041);
#3292=LINE('',#31283,#4042);
#3293=LINE('',#31284,#4043);
#3294=LINE('',#31286,#4044);
#3295=LINE('',#31288,#4045);
#3296=LINE('',#31289,#4046);
#3297=LINE('',#31291,#4047);
#3298=LINE('',#31293,#4048);
#3299=LINE('',#31294,#4049);
#3300=LINE('',#31298,#4050);
#3301=LINE('',#31300,#4051);
#3302=LINE('',#31302,#4052);
#3303=LINE('',#31303,#4053);
#3304=LINE('',#31305,#4054);
#3305=LINE('',#31307,#4055);
#3306=LINE('',#31309,#4056);
#3307=LINE('',#31311,#4057);
#3308=LINE('',#31314,#4058);
#3309=LINE('',#31317,#4059);
#3310=LINE('',#31320,#4060);
#3311=LINE('',#31323,#4061);
#3312=LINE('',#31326,#4062);
#3313=LINE('',#31329,#4063);
#3314=LINE('',#31333,#4064);
#3315=LINE('',#32663,#4065);
#3316=LINE('',#32671,#4066);
#3317=LINE('',#32678,#4067);
#3318=LINE('',#32685,#4068);
#3319=LINE('',#32694,#4069);
#3320=LINE('',#32697,#4070);
#3321=LINE('',#32706,#4071);
#3322=LINE('',#32709,#4072);
#3323=LINE('',#32715,#4073);
#3324=LINE('',#32737,#4074);
#3325=LINE('',#32743,#4075);
#3326=LINE('',#32754,#4076);
#3327=LINE('',#32756,#4077);
#3328=LINE('',#32759,#4078);
#3329=LINE('',#32766,#4079);
#3330=LINE('',#32770,#4080);
#3331=LINE('',#32782,#4081);
#3332=LINE('',#32786,#4082);
#3333=LINE('',#32790,#4083);
#3334=LINE('',#32794,#4084);
#3335=LINE('',#32798,#4085);
#3336=LINE('',#32802,#4086);
#3337=LINE('',#32811,#4087);
#3338=LINE('',#32815,#4088);
#3339=LINE('',#32819,#4089);
#3340=LINE('',#32823,#4090);
#3341=LINE('',#32827,#4091);
#3342=LINE('',#32830,#4092);
#3343=LINE('',#32836,#4093);
#3344=LINE('',#32845,#4094);
#3345=LINE('',#32861,#4095);
#3346=LINE('',#32877,#4096);
#3347=LINE('',#32893,#4097);
#3348=LINE('',#32909,#4098);
#3349=LINE('',#32942,#4099);
#3350=VECTOR('',#11239,1000.);
#3351=VECTOR('',#11242,1000.);
#3352=VECTOR('',#11247,1000.);
#3353=VECTOR('',#11250,1000.);
#3354=VECTOR('',#11255,1000.);
#3355=VECTOR('',#11258,1000.);
#3356=VECTOR('',#11263,1000.);
#3357=VECTOR('',#11266,1000.);
#3358=VECTOR('',#11271,1000.);
#3359=VECTOR('',#11274,1000.);
#3360=VECTOR('',#11279,1000.);
#3361=VECTOR('',#11282,1000.);
#3362=VECTOR('',#11287,1000.);
#3363=VECTOR('',#11290,1000.);
#3364=VECTOR('',#11295,1000.);
#3365=VECTOR('',#11298,1000.);
#3366=VECTOR('',#11303,1000.);
#3367=VECTOR('',#11306,1000.);
#3368=VECTOR('',#11311,1000.);
#3369=VECTOR('',#11314,1000.);
#3370=VECTOR('',#11319,1000.);
#3371=VECTOR('',#11322,1000.);
#3372=VECTOR('',#11327,1000.);
#3373=VECTOR('',#11330,1000.);
#3374=VECTOR('',#11335,1000.);
#3375=VECTOR('',#11338,1000.);
#3376=VECTOR('',#11343,1000.);
#3377=VECTOR('',#11346,1000.);
#3378=VECTOR('',#11351,1000.);
#3379=VECTOR('',#11354,1000.);
#3380=VECTOR('',#11359,1000.);
#3381=VECTOR('',#11362,1000.);
#3382=VECTOR('',#11367,1000.);
#3383=VECTOR('',#11370,1000.);
#3384=VECTOR('',#11375,1000.);
#3385=VECTOR('',#11378,1000.);
#3386=VECTOR('',#11383,1000.);
#3387=VECTOR('',#11386,1000.);
#3388=VECTOR('',#11391,1000.);
#3389=VECTOR('',#11394,1000.);
#3390=VECTOR('',#11399,1000.);
#3391=VECTOR('',#11402,1000.);
#3392=VECTOR('',#11407,1000.);
#3393=VECTOR('',#11410,1000.);
#3394=VECTOR('',#11415,1000.);
#3395=VECTOR('',#11418,1000.);
#3396=VECTOR('',#11423,1000.);
#3397=VECTOR('',#11426,1000.);
#3398=VECTOR('',#11431,1000.);
#3399=VECTOR('',#11434,1000.);
#3400=VECTOR('',#11439,1000.);
#3401=VECTOR('',#11442,1000.);
#3402=VECTOR('',#11447,1000.);
#3403=VECTOR('',#11450,1000.);
#3404=VECTOR('',#11455,1000.);
#3405=VECTOR('',#11458,1000.);
#3406=VECTOR('',#11463,1000.);
#3407=VECTOR('',#11466,1000.);
#3408=VECTOR('',#11471,1000.);
#3409=VECTOR('',#11474,1000.);
#3410=VECTOR('',#11479,1000.);
#3411=VECTOR('',#11482,1000.);
#3412=VECTOR('',#11487,1000.);
#3413=VECTOR('',#11490,1000.);
#3414=VECTOR('',#11495,1000.);
#3415=VECTOR('',#11498,1000.);
#3416=VECTOR('',#11503,1000.);
#3417=VECTOR('',#11506,1000.);
#3418=VECTOR('',#11511,1000.);
#3419=VECTOR('',#11514,1000.);
#3420=VECTOR('',#11519,1000.);
#3421=VECTOR('',#11522,1000.);
#3422=VECTOR('',#11527,1000.);
#3423=VECTOR('',#11530,1000.);
#3424=VECTOR('',#11535,1000.);
#3425=VECTOR('',#11538,1000.);
#3426=VECTOR('',#11543,1000.);
#3427=VECTOR('',#11546,1000.);
#3428=VECTOR('',#11551,1000.);
#3429=VECTOR('',#11554,1000.);
#3430=VECTOR('',#11559,1000.);
#3431=VECTOR('',#11560,1000.);
#3432=VECTOR('',#11561,1000.);
#3433=VECTOR('',#11564,1000.);
#3434=VECTOR('',#11565,1000.);
#3435=VECTOR('',#11568,1000.);
#3436=VECTOR('',#11569,1000.);
#3437=VECTOR('',#11570,1000.);
#3438=VECTOR('',#11573,1000.);
#3439=VECTOR('',#11574,1000.);
#3440=VECTOR('',#11577,1000.);
#3441=VECTOR('',#11578,1000.);
#3442=VECTOR('',#11579,1000.);
#3443=VECTOR('',#11582,1000.);
#3444=VECTOR('',#11583,1000.);
#3445=VECTOR('',#11586,1000.);
#3446=VECTOR('',#11587,1000.);
#3447=VECTOR('',#11588,1000.);
#3448=VECTOR('',#11591,1000.);
#3449=VECTOR('',#11592,1000.);
#3450=VECTOR('',#11595,1000.);
#3451=VECTOR('',#11596,1000.);
#3452=VECTOR('',#11597,1000.);
#3453=VECTOR('',#11600,1000.);
#3454=VECTOR('',#11601,1000.);
#3455=VECTOR('',#11604,1000.);
#3456=VECTOR('',#11605,1000.);
#3457=VECTOR('',#11606,1000.);
#3458=VECTOR('',#11609,1000.);
#3459=VECTOR('',#11610,1000.);
#3460=VECTOR('',#11613,1000.);
#3461=VECTOR('',#11614,1000.);
#3462=VECTOR('',#11615,1000.);
#3463=VECTOR('',#11618,1000.);
#3464=VECTOR('',#11619,1000.);
#3465=VECTOR('',#11622,1000.);
#3466=VECTOR('',#11623,1000.);
#3467=VECTOR('',#11624,1000.);
#3468=VECTOR('',#11627,1000.);
#3469=VECTOR('',#11628,1000.);
#3470=VECTOR('',#11631,1000.);
#3471=VECTOR('',#11632,1000.);
#3472=VECTOR('',#11633,1000.);
#3473=VECTOR('',#11636,1000.);
#3474=VECTOR('',#11637,1000.);
#3475=VECTOR('',#11640,1000.);
#3476=VECTOR('',#11641,1000.);
#3477=VECTOR('',#11642,1000.);
#3478=VECTOR('',#11645,1000.);
#3479=VECTOR('',#11646,1000.);
#3480=VECTOR('',#11649,1000.);
#3481=VECTOR('',#11650,1000.);
#3482=VECTOR('',#11651,1000.);
#3483=VECTOR('',#11654,1000.);
#3484=VECTOR('',#11655,1000.);
#3485=VECTOR('',#11658,1000.);
#3486=VECTOR('',#11659,1000.);
#3487=VECTOR('',#11660,1000.);
#3488=VECTOR('',#11663,1000.);
#3489=VECTOR('',#11664,1000.);
#3490=VECTOR('',#11667,1000.);
#3491=VECTOR('',#11668,1000.);
#3492=VECTOR('',#11669,1000.);
#3493=VECTOR('',#11672,1000.);
#3494=VECTOR('',#11673,1000.);
#3495=VECTOR('',#11676,1000.);
#3496=VECTOR('',#11677,1000.);
#3497=VECTOR('',#11678,1000.);
#3498=VECTOR('',#11681,1000.);
#3499=VECTOR('',#11682,1000.);
#3500=VECTOR('',#11685,1000.);
#3501=VECTOR('',#11686,1000.);
#3502=VECTOR('',#11687,1000.);
#3503=VECTOR('',#11690,1000.);
#3504=VECTOR('',#11691,1000.);
#3505=VECTOR('',#11694,1000.);
#3506=VECTOR('',#11695,1000.);
#3507=VECTOR('',#11696,1000.);
#3508=VECTOR('',#11699,1000.);
#3509=VECTOR('',#11700,1000.);
#3510=VECTOR('',#11703,1000.);
#3511=VECTOR('',#11704,1000.);
#3512=VECTOR('',#11705,1000.);
#3513=VECTOR('',#11708,1000.);
#3514=VECTOR('',#11709,1000.);
#3515=VECTOR('',#11712,1000.);
#3516=VECTOR('',#11713,1000.);
#3517=VECTOR('',#11714,1000.);
#3518=VECTOR('',#11717,1000.);
#3519=VECTOR('',#11718,1000.);
#3520=VECTOR('',#11721,1000.);
#3521=VECTOR('',#11722,1000.);
#3522=VECTOR('',#11723,1000.);
#3523=VECTOR('',#11726,1000.);
#3524=VECTOR('',#11727,1000.);
#3525=VECTOR('',#11730,1000.);
#3526=VECTOR('',#11731,1000.);
#3527=VECTOR('',#11732,1000.);
#3528=VECTOR('',#11735,1000.);
#3529=VECTOR('',#11736,1000.);
#3530=VECTOR('',#11739,1000.);
#3531=VECTOR('',#11740,1000.);
#3532=VECTOR('',#11741,1000.);
#3533=VECTOR('',#11744,1000.);
#3534=VECTOR('',#11745,1000.);
#3535=VECTOR('',#11748,1000.);
#3536=VECTOR('',#11749,1000.);
#3537=VECTOR('',#11750,1000.);
#3538=VECTOR('',#11753,1000.);
#3539=VECTOR('',#11754,1000.);
#3540=VECTOR('',#11757,1000.);
#3541=VECTOR('',#11758,1000.);
#3542=VECTOR('',#11759,1000.);
#3543=VECTOR('',#11762,1000.);
#3544=VECTOR('',#11763,1000.);
#3545=VECTOR('',#11766,1000.);
#3546=VECTOR('',#11767,1000.);
#3547=VECTOR('',#11768,1000.);
#3548=VECTOR('',#11771,1000.);
#3549=VECTOR('',#11772,1000.);
#3550=VECTOR('',#11775,1000.);
#3551=VECTOR('',#11776,1000.);
#3552=VECTOR('',#11777,1000.);
#3553=VECTOR('',#11780,1000.);
#3554=VECTOR('',#11781,1000.);
#3555=VECTOR('',#11784,1000.);
#3556=VECTOR('',#11785,1000.);
#3557=VECTOR('',#11786,1000.);
#3558=VECTOR('',#11789,1000.);
#3559=VECTOR('',#11790,1000.);
#3560=VECTOR('',#11793,1000.);
#3561=VECTOR('',#11794,1000.);
#3562=VECTOR('',#11795,1000.);
#3563=VECTOR('',#11798,1000.);
#3564=VECTOR('',#11799,1000.);
#3565=VECTOR('',#11802,1000.);
#3566=VECTOR('',#11803,1000.);
#3567=VECTOR('',#11804,1000.);
#3568=VECTOR('',#11807,1000.);
#3569=VECTOR('',#11808,1000.);
#3570=VECTOR('',#11811,1000.);
#3571=VECTOR('',#11812,1000.);
#3572=VECTOR('',#11813,1000.);
#3573=VECTOR('',#11816,1000.);
#3574=VECTOR('',#11817,1000.);
#3575=VECTOR('',#11820,1000.);
#3576=VECTOR('',#11821,1000.);
#3577=VECTOR('',#11822,1000.);
#3578=VECTOR('',#11825,1000.);
#3579=VECTOR('',#11826,1000.);
#3580=VECTOR('',#11829,1000.);
#3581=VECTOR('',#11830,1000.);
#3582=VECTOR('',#11831,1000.);
#3583=VECTOR('',#11834,1000.);
#3584=VECTOR('',#11835,1000.);
#3585=VECTOR('',#11838,1000.);
#3586=VECTOR('',#11839,1000.);
#3587=VECTOR('',#11840,1000.);
#3588=VECTOR('',#11843,1000.);
#3589=VECTOR('',#11844,1000.);
#3590=VECTOR('',#11847,1000.);
#3591=VECTOR('',#11848,1000.);
#3592=VECTOR('',#11849,1000.);
#3593=VECTOR('',#11852,1000.);
#3594=VECTOR('',#11853,1000.);
#3595=VECTOR('',#11856,1000.);
#3596=VECTOR('',#11857,1000.);
#3597=VECTOR('',#11858,1000.);
#3598=VECTOR('',#11861,1000.);
#3599=VECTOR('',#11862,1000.);
#3600=VECTOR('',#11865,1000.);
#3601=VECTOR('',#11866,1000.);
#3602=VECTOR('',#11867,1000.);
#3603=VECTOR('',#11870,1000.);
#3604=VECTOR('',#11871,1000.);
#3605=VECTOR('',#11874,1000.);
#3606=VECTOR('',#11875,1000.);
#3607=VECTOR('',#11876,1000.);
#3608=VECTOR('',#11879,1000.);
#3609=VECTOR('',#11880,1000.);
#3610=VECTOR('',#11883,1000.);
#3611=VECTOR('',#11884,1000.);
#3612=VECTOR('',#11885,1000.);
#3613=VECTOR('',#11888,1000.);
#3614=VECTOR('',#11889,1000.);
#3615=VECTOR('',#11892,1000.);
#3616=VECTOR('',#11893,1000.);
#3617=VECTOR('',#11894,1000.);
#3618=VECTOR('',#11897,1000.);
#3619=VECTOR('',#11898,1000.);
#3620=VECTOR('',#11901,1000.);
#3621=VECTOR('',#11902,1000.);
#3622=VECTOR('',#11903,1000.);
#3623=VECTOR('',#11906,1000.);
#3624=VECTOR('',#11907,1000.);
#3625=VECTOR('',#11910,1000.);
#3626=VECTOR('',#11911,1000.);
#3627=VECTOR('',#11912,1000.);
#3628=VECTOR('',#11915,1000.);
#3629=VECTOR('',#11916,1000.);
#3630=VECTOR('',#11937,10.75);
#3631=VECTOR('',#11958,20.);
#3632=VECTOR('',#11989,8.35);
#3633=VECTOR('',#11998,8.35);
#3634=VECTOR('',#12007,3.1);
#3635=VECTOR('',#12010,1000.);
#3636=VECTOR('',#12011,1000.);
#3637=VECTOR('',#12012,1000.);
#3638=VECTOR('',#12013,1000.);
#3639=VECTOR('',#12016,1000.);
#3640=VECTOR('',#12017,1000.);
#3641=VECTOR('',#12018,1000.);
#3642=VECTOR('',#12021,1000.);
#3643=VECTOR('',#12022,1000.);
#3644=VECTOR('',#12025,1000.);
#3645=VECTOR('',#12026,1000.);
#3646=VECTOR('',#12029,1000.);
#3647=VECTOR('',#12038,1000.);
#3648=VECTOR('',#12039,1000.);
#3649=VECTOR('',#12040,1000.);
#3650=VECTOR('',#12043,1000.);
#3651=VECTOR('',#12044,1000.);
#3652=VECTOR('',#12047,1000.);
#3653=VECTOR('',#12048,1000.);
#3654=VECTOR('',#12051,1000.);
#3655=VECTOR('',#12052,1000.);
#3656=VECTOR('',#12055,1000.);
#3657=VECTOR('',#12056,1000.);
#3658=VECTOR('',#12059,1000.);
#3659=VECTOR('',#12060,1000.);
#3660=VECTOR('',#12063,1000.);
#3661=VECTOR('',#12064,1000.);
#3662=VECTOR('',#12069,1000.);
#3663=VECTOR('',#12074,17.85);
#3664=VECTOR('',#12075,1000.);
#3665=VECTOR('',#12076,17.85);
#3666=VECTOR('',#12081,1000.);
#3667=VECTOR('',#12094,20.);
#3668=VECTOR('',#12105,15.);
#3669=VECTOR('',#12122,16.5);
#3670=VECTOR('',#12131,17.85);
#3671=VECTOR('',#12136,3.);
#3672=VECTOR('',#12141,5.);
#3673=VECTOR('',#12142,1000.);
#3674=VECTOR('',#12143,5.);
#3675=VECTOR('',#12148,1000.);
#3676=VECTOR('',#12155,1000.);
#3677=VECTOR('',#12156,1000.);
#3678=VECTOR('',#12161,1000.);
#3679=VECTOR('',#12164,1000.);
#3680=VECTOR('',#12173,3.);
#3681=VECTOR('',#12178,2.8);
#3682=VECTOR('',#12183,6.08697438789325);
#3683=VECTOR('',#12190,19.5);
#3684=VECTOR('',#12193,5.);
#3685=VECTOR('',#12198,1000.);
#3686=VECTOR('',#12201,1000.);
#3687=VECTOR('',#12208,1000.);
#3688=VECTOR('',#12211,1000.);
#3689=VECTOR('',#12214,1000.);
#3690=VECTOR('',#12215,1000.);
#3691=VECTOR('',#12216,1000.);
#3692=VECTOR('',#12219,1000.);
#3693=VECTOR('',#12220,1000.);
#3694=VECTOR('',#12221,1000.);
#3695=VECTOR('',#12224,1000.);
#3696=VECTOR('',#12225,1000.);
#3697=VECTOR('',#12226,1000.);
#3698=VECTOR('',#12227,1000.);
#3699=VECTOR('',#12228,1000.);
#3700=VECTOR('',#12229,1000.);
#3701=VECTOR('',#12230,1000.);
#3702=VECTOR('',#12231,1000.);
#3703=VECTOR('',#12232,1000.);
#3704=VECTOR('',#12233,1000.);
#3705=VECTOR('',#12234,1000.);
#3706=VECTOR('',#12235,1000.);
#3707=VECTOR('',#12236,1000.);
#3708=VECTOR('',#12237,1000.);
#3709=VECTOR('',#12238,1000.);
#3710=VECTOR('',#12239,1000.);
#3711=VECTOR('',#12244,1000.);
#3712=VECTOR('',#12245,1000.);
#3713=VECTOR('',#12246,1000.);
#3714=VECTOR('',#12247,1000.);
#3715=VECTOR('',#12248,1000.);
#3716=VECTOR('',#12249,1000.);
#3717=VECTOR('',#12250,1000.);
#3718=VECTOR('',#12251,1000.);
#3719=VECTOR('',#12252,1000.);
#3720=VECTOR('',#12253,1000.);
#3721=VECTOR('',#12254,1000.);
#3722=VECTOR('',#12255,1000.);
#3723=VECTOR('',#12256,1000.);
#3724=VECTOR('',#12257,1000.);
#3725=VECTOR('',#12258,1000.);
#3726=VECTOR('',#12259,1000.);
#3727=VECTOR('',#12266,3.);
#3728=VECTOR('',#12273,1000.);
#3729=VECTOR('',#12276,1000.);
#3730=VECTOR('',#12279,1000.);
#3731=VECTOR('',#12282,1000.);
#3732=VECTOR('',#12285,1000.);
#3733=VECTOR('',#12288,1000.);
#3734=VECTOR('',#12291,1000.);
#3735=VECTOR('',#12296,1000.);
#3736=VECTOR('',#12299,1000.);
#3737=VECTOR('',#12302,1000.);
#3738=VECTOR('',#12305,1000.);
#3739=VECTOR('',#12308,1000.);
#3740=VECTOR('',#12311,1000.);
#3741=VECTOR('',#12314,1000.);
#3742=VECTOR('',#12319,3.5);
#3743=VECTOR('',#12322,3.);
#3744=VECTOR('',#12331,3.);
#3745=VECTOR('',#12344,3.);
#3746=VECTOR('',#12347,2.5);
#3747=VECTOR('',#12358,5.);
#3748=VECTOR('',#12371,15.);
#3749=VECTOR('',#12382,1000.);
#3750=VECTOR('',#12389,1000.);
#3751=VECTOR('',#12396,1000.);
#3752=VECTOR('',#12397,1000.);
#3753=VECTOR('',#12400,1000.);
#3754=VECTOR('',#12401,1000.);
#3755=VECTOR('',#12402,1000.);
#3756=VECTOR('',#12405,1000.);
#3757=VECTOR('',#12408,1000.);
#3758=VECTOR('',#12411,1000.);
#3759=VECTOR('',#12412,1000.);
#3760=VECTOR('',#12413,1000.);
#3761=VECTOR('',#12428,2.8);
#3762=VECTOR('',#12433,4.50000000000001);
#3763=VECTOR('',#12436,14.5);
#3764=VECTOR('',#12527,11.1);
#3765=VECTOR('',#12528,1000.);
#3766=VECTOR('',#12529,11.1);
#3767=VECTOR('',#12532,1000.);
#3768=VECTOR('',#12533,1000.);
#3769=VECTOR('',#12534,1000.);
#3770=VECTOR('',#12535,1000.);
#3771=VECTOR('',#12536,1000.);
#3772=VECTOR('',#12537,1000.);
#3773=VECTOR('',#12538,1000.);
#3774=VECTOR('',#12539,1000.);
#3775=VECTOR('',#12540,1000.);
#3776=VECTOR('',#12541,1000.);
#3777=VECTOR('',#12542,1000.);
#3778=VECTOR('',#12543,1000.);
#3779=VECTOR('',#12544,1000.);
#3780=VECTOR('',#12545,1000.);
#3781=VECTOR('',#12546,1000.);
#3782=VECTOR('',#12547,1000.);
#3783=VECTOR('',#12548,1000.);
#3784=VECTOR('',#12549,1000.);
#3785=VECTOR('',#12550,1000.);
#3786=VECTOR('',#12555,11.1);
#3787=VECTOR('',#12556,11.1);
#3788=VECTOR('',#12565,11.1);
#3789=VECTOR('',#12566,11.1);
#3790=VECTOR('',#12585,9.2);
#3791=VECTOR('',#12586,9.2);
#3792=VECTOR('',#12587,9.2);
#3793=VECTOR('',#12594,3.09999999999999);
#3794=VECTOR('',#12597,3.09999999999999);
#3795=VECTOR('',#12600,2.);
#3796=VECTOR('',#12603,2.);
#3797=VECTOR('',#12674,9.2);
#3798=VECTOR('',#12677,9.70000000000007);
#3799=VECTOR('',#12680,10.6);
#3800=VECTOR('',#12683,11.1);
#3801=VECTOR('',#12690,9.1);
#3802=VECTOR('',#12691,9.1);
#3803=VECTOR('',#12706,2.125);
#3804=VECTOR('',#12713,2.125);
#3805=VECTOR('',#12718,3.5);
#3806=VECTOR('',#12729,5.);
#3807=VECTOR('',#12748,3.);
#3808=VECTOR('',#12753,2.4455);
#3809=VECTOR('',#12758,1000.);
#3810=VECTOR('',#12759,1000.);
#3811=VECTOR('',#12760,1000.);
#3812=VECTOR('',#12761,1000.);
#3813=VECTOR('',#12762,1000.);
#3814=VECTOR('',#12763,1000.);
#3815=VECTOR('',#12766,1000.);
#3816=VECTOR('',#12767,1000.);
#3817=VECTOR('',#12768,1000.);
#3818=VECTOR('',#12771,1000.);
#3819=VECTOR('',#12772,1000.);
#3820=VECTOR('',#12775,1000.);
#3821=VECTOR('',#12776,1000.);
#3822=VECTOR('',#12779,1000.);
#3823=VECTOR('',#12780,1000.);
#3824=VECTOR('',#12783,1000.);
#3825=VECTOR('',#12784,1000.);
#3826=VECTOR('',#12787,1000.);
#3827=VECTOR('',#12796,1000.);
#3828=VECTOR('',#12799,1000.);
#3829=VECTOR('',#12814,9.15);
#3830=VECTOR('',#12829,6.75);
#3831=VECTOR('',#12834,1000.);
#3832=VECTOR('',#12835,1000.);
#3833=VECTOR('',#12836,1000.);
#3834=VECTOR('',#12837,1000.);
#3835=VECTOR('',#12840,1000.);
#3836=VECTOR('',#12841,1000.);
#3837=VECTOR('',#12842,1000.);
#3838=VECTOR('',#12845,1000.);
#3839=VECTOR('',#12846,1000.);
#3840=VECTOR('',#12849,1000.);
#3841=VECTOR('',#12850,1000.);
#3842=VECTOR('',#12853,1000.);
#3843=VECTOR('',#12866,1000.);
#3844=VECTOR('',#12867,1000.);
#3845=VECTOR('',#12868,1000.);
#3846=VECTOR('',#12869,1000.);
#3847=VECTOR('',#12870,1000.);
#3848=VECTOR('',#12871,1000.);
#3849=VECTOR('',#12872,1000.);
#3850=VECTOR('',#12873,1000.);
#3851=VECTOR('',#12874,1000.);
#3852=VECTOR('',#12875,1000.);
#3853=VECTOR('',#12876,1000.);
#3854=VECTOR('',#12877,1000.);
#3855=VECTOR('',#12878,1000.);
#3856=VECTOR('',#12879,1000.);
#3857=VECTOR('',#12880,1000.);
#3858=VECTOR('',#12881,1000.);
#3859=VECTOR('',#12884,1000.);
#3860=VECTOR('',#12885,1000.);
#3861=VECTOR('',#12886,1000.);
#3862=VECTOR('',#12889,1000.);
#3863=VECTOR('',#12890,1000.);
#3864=VECTOR('',#12893,1000.);
#3865=VECTOR('',#12894,1000.);
#3866=VECTOR('',#12897,1000.);
#3867=VECTOR('',#12900,1000.);
#3868=VECTOR('',#12901,1000.);
#3869=VECTOR('',#12902,1000.);
#3870=VECTOR('',#12903,1000.);
#3871=VECTOR('',#12904,1000.);
#3872=VECTOR('',#12905,1000.);
#3873=VECTOR('',#12906,1000.);
#3874=VECTOR('',#12907,1000.);
#3875=VECTOR('',#12908,1000.);
#3876=VECTOR('',#12909,1000.);
#3877=VECTOR('',#12910,1000.);
#3878=VECTOR('',#12911,1000.);
#3879=VECTOR('',#12914,1000.);
#3880=VECTOR('',#12915,1000.);
#3881=VECTOR('',#12916,1000.);
#3882=VECTOR('',#12919,1000.);
#3883=VECTOR('',#12920,1000.);
#3884=VECTOR('',#12923,1000.);
#3885=VECTOR('',#12924,1000.);
#3886=VECTOR('',#12927,1000.);
#3887=VECTOR('',#12928,1000.);
#3888=VECTOR('',#12931,1000.);
#3889=VECTOR('',#12932,1000.);
#3890=VECTOR('',#12935,1000.);
#3891=VECTOR('',#12936,1000.);
#3892=VECTOR('',#12939,1000.);
#3893=VECTOR('',#12940,1000.);
#3894=VECTOR('',#12943,1000.);
#3895=VECTOR('',#12944,1000.);
#3896=VECTOR('',#12947,1000.);
#3897=VECTOR('',#12948,1000.);
#3898=VECTOR('',#12951,1000.);
#3899=VECTOR('',#12952,1000.);
#3900=VECTOR('',#12955,1000.);
#3901=VECTOR('',#12956,1000.);
#3902=VECTOR('',#12959,1000.);
#3903=VECTOR('',#12964,1000.);
#3904=VECTOR('',#12965,1000.);
#3905=VECTOR('',#12966,1000.);
#3906=VECTOR('',#12969,1000.);
#3907=VECTOR('',#12970,1000.);
#3908=VECTOR('',#12973,1000.);
#3909=VECTOR('',#12974,1000.);
#3910=VECTOR('',#12977,1000.);
#3911=VECTOR('',#12978,1000.);
#3912=VECTOR('',#12981,1000.);
#3913=VECTOR('',#12982,1000.);
#3914=VECTOR('',#12985,1000.);
#3915=VECTOR('',#12986,1000.);
#3916=VECTOR('',#12989,1000.);
#3917=VECTOR('',#12990,1000.);
#3918=VECTOR('',#12993,1000.);
#3919=VECTOR('',#12994,1000.);
#3920=VECTOR('',#12997,1000.);
#3921=VECTOR('',#12998,1000.);
#3922=VECTOR('',#13001,1000.);
#3923=VECTOR('',#13002,1000.);
#3924=VECTOR('',#13005,1000.);
#3925=VECTOR('',#13006,1000.);
#3926=VECTOR('',#13009,1000.);
#3927=VECTOR('',#13032,8.925);
#3928=VECTOR('',#13055,9.15);
#3929=VECTOR('',#13058,7.25);
#3930=VECTOR('',#13093,3.);
#3931=VECTOR('',#13102,3.75);
#3932=VECTOR('',#13115,2.4);
#3933=VECTOR('',#13126,3.);
#3934=VECTOR('',#13135,1000.);
#3935=VECTOR('',#13138,1000.);
#3936=VECTOR('',#13141,1000.);
#3937=VECTOR('',#13144,1000.);
#3938=VECTOR('',#13149,1000.);
#3939=VECTOR('',#13152,1000.);
#3940=VECTOR('',#13157,1000.);
#3941=VECTOR('',#13160,1000.);
#3942=VECTOR('',#13169,1000.);
#3943=VECTOR('',#13172,1000.);
#3944=VECTOR('',#13175,1000.);
#3945=VECTOR('',#13178,1000.);
#3946=VECTOR('',#13183,1000.);
#3947=VECTOR('',#13186,1000.);
#3948=VECTOR('',#13191,1000.);
#3949=VECTOR('',#13194,1000.);
#3950=VECTOR('',#13199,1000.);
#3951=VECTOR('',#13202,1000.);
#3952=VECTOR('',#13235,14.);
#3953=VECTOR('',#13242,14.);
#3954=VECTOR('',#13247,1000.);
#3955=VECTOR('',#13248,1000.);
#3956=VECTOR('',#13263,13.);
#3957=VECTOR('',#13266,13.);
#3958=VECTOR('',#13275,16.);
#3959=VECTOR('',#13282,16.);
#3960=VECTOR('',#13289,11.35);
#3961=VECTOR('',#13292,1.87499999999999);
#3962=VECTOR('',#13295,1.87500000000001);
#3963=VECTOR('',#13298,1.875);
#3964=VECTOR('',#13301,1.875);
#3965=VECTOR('',#13304,1.875);
#3966=VECTOR('',#13309,15.);
#3967=VECTOR('',#13312,13.5);
#3968=VECTOR('',#13319,15.5);
#3969=VECTOR('',#13326,1000.);
#3970=VECTOR('',#13329,1000.);
#3971=VECTOR('',#13332,1000.);
#3972=VECTOR('',#13335,1000.);
#3973=VECTOR('',#13338,1000.);
#3974=VECTOR('',#13341,1000.);
#3975=VECTOR('',#13344,1000.);
#3976=VECTOR('',#13347,1000.);
#3977=VECTOR('',#13350,1000.);
#3978=VECTOR('',#13353,1000.);
#3979=VECTOR('',#13356,1000.);
#3980=VECTOR('',#13359,1000.);
#3981=VECTOR('',#13362,1000.);
#3982=VECTOR('',#13365,1000.);
#3983=VECTOR('',#13368,1000.);
#3984=VECTOR('',#13371,1000.);
#3985=VECTOR('',#13374,1000.);
#3986=VECTOR('',#13377,1000.);
#3987=VECTOR('',#13380,1000.);
#3988=VECTOR('',#13383,1000.);
#3989=VECTOR('',#13468,1000.);
#3990=VECTOR('',#13469,1000.);
#3991=VECTOR('',#13470,1000.);
#3992=VECTOR('',#13471,1000.);
#3993=VECTOR('',#13472,1000.);
#3994=VECTOR('',#13473,1000.);
#3995=VECTOR('',#13474,1000.);
#3996=VECTOR('',#13475,1000.);
#3997=VECTOR('',#13476,1000.);
#3998=VECTOR('',#13477,1000.);
#3999=VECTOR('',#13478,1000.);
#4000=VECTOR('',#13479,1000.);
#4001=VECTOR('',#13480,1000.);
#4002=VECTOR('',#13481,1000.);
#4003=VECTOR('',#13482,1000.);
#4004=VECTOR('',#13483,1000.);
#4005=VECTOR('',#13484,1000.);
#4006=VECTOR('',#13485,1000.);
#4007=VECTOR('',#13486,1000.);
#4008=VECTOR('',#13487,1000.);
#4009=VECTOR('',#13488,1000.);
#4010=VECTOR('',#13489,1000.);
#4011=VECTOR('',#13490,1000.);
#4012=VECTOR('',#13491,1000.);
#4013=VECTOR('',#13494,1000.);
#4014=VECTOR('',#13495,1000.);
#4015=VECTOR('',#13496,1000.);
#4016=VECTOR('',#13499,1000.);
#4017=VECTOR('',#13500,1000.);
#4018=VECTOR('',#13501,1000.);
#4019=VECTOR('',#13504,1000.);
#4020=VECTOR('',#13505,1000.);
#4021=VECTOR('',#13506,1000.);
#4022=VECTOR('',#13509,1000.);
#4023=VECTOR('',#13510,1000.);
#4024=VECTOR('',#13511,1000.);
#4025=VECTOR('',#13514,1000.);
#4026=VECTOR('',#13515,1000.);
#4027=VECTOR('',#13518,1000.);
#4028=VECTOR('',#13519,1000.);
#4029=VECTOR('',#13520,1000.);
#4030=VECTOR('',#13527,4.5);
#4031=VECTOR('',#13534,15.);
#4032=VECTOR('',#13539,1000.);
#4033=VECTOR('',#13540,1000.);
#4034=VECTOR('',#13541,1000.);
#4035=VECTOR('',#13542,1000.);
#4036=VECTOR('',#13543,1000.);
#4037=VECTOR('',#13544,1000.);
#4038=VECTOR('',#13545,1000.);
#4039=VECTOR('',#13546,1000.);
#4040=VECTOR('',#13547,1000.);
#4041=VECTOR('',#13548,1000.);
#4042=VECTOR('',#13549,1000.);
#4043=VECTOR('',#13550,1000.);
#4044=VECTOR('',#13551,1000.);
#4045=VECTOR('',#13552,1000.);
#4046=VECTOR('',#13553,1000.);
#4047=VECTOR('',#13554,1000.);
#4048=VECTOR('',#13555,1000.);
#4049=VECTOR('',#13556,1000.);
#4050=VECTOR('',#13561,1000.);
#4051=VECTOR('',#13564,1000.);
#4052=VECTOR('',#13567,1000.);
#4053=VECTOR('',#13568,1000.);
#4054=VECTOR('',#13571,1000.);
#4055=VECTOR('',#13574,1000.);
#4056=VECTOR('',#13577,1000.);
#4057=VECTOR('',#13580,1000.);
#4058=VECTOR('',#13585,1000.);
#4059=VECTOR('',#13590,1000.);
#4060=VECTOR('',#13595,1000.);
#4061=VECTOR('',#13600,1000.);
#4062=VECTOR('',#13605,1000.);
#4063=VECTOR('',#13610,6.50000000000001);
#4064=VECTOR('',#13617,13.8985);
#4065=VECTOR('',#13650,19.);
#4066=VECTOR('',#13661,16.);
#4067=VECTOR('',#13670,13.1);
#4068=VECTOR('',#13679,15.1);
#4069=VECTOR('',#13690,14.1);
#4070=VECTOR('',#13693,14.1);
#4071=VECTOR('',#13704,13.1);
#4072=VECTOR('',#13707,13.1);
#4073=VECTOR('',#13716,16.1);
#4074=VECTOR('',#13751,11.);
#4075=VECTOR('',#13758,15.75);
#4076=VECTOR('',#13771,13.5);
#4077=VECTOR('',#13774,15.25);
#4078=VECTOR('',#13777,12.3985);
#4079=VECTOR('',#13786,9.);
#4080=VECTOR('',#13791,9.);
#4081=VECTOR('',#13808,1000.);
#4082=VECTOR('',#13811,1000.);
#4083=VECTOR('',#13814,1000.);
#4084=VECTOR('',#13817,1000.);
#4085=VECTOR('',#13820,1000.);
#4086=VECTOR('',#13823,1000.);
#4087=VECTOR('',#13832,1000.);
#4088=VECTOR('',#13835,1000.);
#4089=VECTOR('',#13838,1000.);
#4090=VECTOR('',#13841,1000.);
#4091=VECTOR('',#13844,1000.);
#4092=VECTOR('',#13847,1000.);
#4093=VECTOR('',#13852,1000.);
#4094=VECTOR('',#13853,1000.);
#4095=VECTOR('',#13856,1000.);
#4096=VECTOR('',#13859,1000.);
#4097=VECTOR('',#13862,1000.);
#4098=VECTOR('',#13865,1000.);
#4099=VECTOR('',#13894,3.5);
#4100=VERTEX_POINT('',#13918);
#4101=VERTEX_POINT('',#13919);
#4102=VERTEX_POINT('',#13921);
#4103=VERTEX_POINT('',#13923);
#4104=VERTEX_POINT('',#13927);
#4105=VERTEX_POINT('',#13928);
#4106=VERTEX_POINT('',#13930);
#4107=VERTEX_POINT('',#13932);
#4108=VERTEX_POINT('',#13936);
#4109=VERTEX_POINT('',#13937);
#4110=VERTEX_POINT('',#13939);
#4111=VERTEX_POINT('',#13941);
#4112=VERTEX_POINT('',#13945);
#4113=VERTEX_POINT('',#13946);
#4114=VERTEX_POINT('',#13948);
#4115=VERTEX_POINT('',#13950);
#4116=VERTEX_POINT('',#13954);
#4117=VERTEX_POINT('',#13955);
#4118=VERTEX_POINT('',#13957);
#4119=VERTEX_POINT('',#13959);
#4120=VERTEX_POINT('',#13963);
#4121=VERTEX_POINT('',#13964);
#4122=VERTEX_POINT('',#13966);
#4123=VERTEX_POINT('',#13968);
#4124=VERTEX_POINT('',#13972);
#4125=VERTEX_POINT('',#13973);
#4126=VERTEX_POINT('',#13975);
#4127=VERTEX_POINT('',#13977);
#4128=VERTEX_POINT('',#13981);
#4129=VERTEX_POINT('',#13982);
#4130=VERTEX_POINT('',#13984);
#4131=VERTEX_POINT('',#13986);
#4132=VERTEX_POINT('',#13990);
#4133=VERTEX_POINT('',#13991);
#4134=VERTEX_POINT('',#13993);
#4135=VERTEX_POINT('',#13995);
#4136=VERTEX_POINT('',#13999);
#4137=VERTEX_POINT('',#14000);
#4138=VERTEX_POINT('',#14002);
#4139=VERTEX_POINT('',#14004);
#4140=VERTEX_POINT('',#14008);
#4141=VERTEX_POINT('',#14009);
#4142=VERTEX_POINT('',#14011);
#4143=VERTEX_POINT('',#14013);
#4144=VERTEX_POINT('',#14017);
#4145=VERTEX_POINT('',#14018);
#4146=VERTEX_POINT('',#14020);
#4147=VERTEX_POINT('',#14022);
#4148=VERTEX_POINT('',#14026);
#4149=VERTEX_POINT('',#14027);
#4150=VERTEX_POINT('',#14029);
#4151=VERTEX_POINT('',#14031);
#4152=VERTEX_POINT('',#14035);
#4153=VERTEX_POINT('',#14036);
#4154=VERTEX_POINT('',#14038);
#4155=VERTEX_POINT('',#14040);
#4156=VERTEX_POINT('',#14044);
#4157=VERTEX_POINT('',#14045);
#4158=VERTEX_POINT('',#14047);
#4159=VERTEX_POINT('',#14049);
#4160=VERTEX_POINT('',#14053);
#4161=VERTEX_POINT('',#14054);
#4162=VERTEX_POINT('',#14056);
#4163=VERTEX_POINT('',#14058);
#4164=VERTEX_POINT('',#14062);
#4165=VERTEX_POINT('',#14063);
#4166=VERTEX_POINT('',#14065);
#4167=VERTEX_POINT('',#14067);
#4168=VERTEX_POINT('',#14071);
#4169=VERTEX_POINT('',#14072);
#4170=VERTEX_POINT('',#14074);
#4171=VERTEX_POINT('',#14076);
#4172=VERTEX_POINT('',#14080);
#4173=VERTEX_POINT('',#14081);
#4174=VERTEX_POINT('',#14083);
#4175=VERTEX_POINT('',#14085);
#4176=VERTEX_POINT('',#14089);
#4177=VERTEX_POINT('',#14090);
#4178=VERTEX_POINT('',#14092);
#4179=VERTEX_POINT('',#14094);
#4180=VERTEX_POINT('',#14098);
#4181=VERTEX_POINT('',#14099);
#4182=VERTEX_POINT('',#14101);
#4183=VERTEX_POINT('',#14103);
#4184=VERTEX_POINT('',#14107);
#4185=VERTEX_POINT('',#14108);
#4186=VERTEX_POINT('',#14110);
#4187=VERTEX_POINT('',#14112);
#4188=VERTEX_POINT('',#14116);
#4189=VERTEX_POINT('',#14117);
#4190=VERTEX_POINT('',#14119);
#4191=VERTEX_POINT('',#14121);
#4192=VERTEX_POINT('',#14125);
#4193=VERTEX_POINT('',#14126);
#4194=VERTEX_POINT('',#14128);
#4195=VERTEX_POINT('',#14130);
#4196=VERTEX_POINT('',#14134);
#4197=VERTEX_POINT('',#14135);
#4198=VERTEX_POINT('',#14137);
#4199=VERTEX_POINT('',#14139);
#4200=VERTEX_POINT('',#14143);
#4201=VERTEX_POINT('',#14144);
#4202=VERTEX_POINT('',#14146);
#4203=VERTEX_POINT('',#14148);
#4204=VERTEX_POINT('',#14152);
#4205=VERTEX_POINT('',#14153);
#4206=VERTEX_POINT('',#14155);
#4207=VERTEX_POINT('',#14157);
#4208=VERTEX_POINT('',#14161);
#4209=VERTEX_POINT('',#14162);
#4210=VERTEX_POINT('',#14164);
#4211=VERTEX_POINT('',#14166);
#4212=VERTEX_POINT('',#14170);
#4213=VERTEX_POINT('',#14171);
#4214=VERTEX_POINT('',#14173);
#4215=VERTEX_POINT('',#14175);
#4216=VERTEX_POINT('',#14179);
#4217=VERTEX_POINT('',#14180);
#4218=VERTEX_POINT('',#14182);
#4219=VERTEX_POINT('',#14184);
#4220=VERTEX_POINT('',#14188);
#4221=VERTEX_POINT('',#14189);
#4222=VERTEX_POINT('',#14191);
#4223=VERTEX_POINT('',#14193);
#4224=VERTEX_POINT('',#14197);
#4225=VERTEX_POINT('',#14198);
#4226=VERTEX_POINT('',#14200);
#4227=VERTEX_POINT('',#14202);
#4228=VERTEX_POINT('',#14206);
#4229=VERTEX_POINT('',#14207);
#4230=VERTEX_POINT('',#14209);
#4231=VERTEX_POINT('',#14211);
#4232=VERTEX_POINT('',#14215);
#4233=VERTEX_POINT('',#14216);
#4234=VERTEX_POINT('',#14218);
#4235=VERTEX_POINT('',#14220);
#4236=VERTEX_POINT('',#14224);
#4237=VERTEX_POINT('',#14225);
#4238=VERTEX_POINT('',#14227);
#4239=VERTEX_POINT('',#14229);
#4240=VERTEX_POINT('',#14233);
#4241=VERTEX_POINT('',#14234);
#4242=VERTEX_POINT('',#14236);
#4243=VERTEX_POINT('',#14238);
#4244=VERTEX_POINT('',#14242);
#4245=VERTEX_POINT('',#14243);
#4246=VERTEX_POINT('',#14245);
#4247=VERTEX_POINT('',#14247);
#4248=VERTEX_POINT('',#14251);
#4249=VERTEX_POINT('',#14252);
#4250=VERTEX_POINT('',#14254);
#4251=VERTEX_POINT('',#14256);
#4252=VERTEX_POINT('',#14260);
#4253=VERTEX_POINT('',#14261);
#4254=VERTEX_POINT('',#14263);
#4255=VERTEX_POINT('',#14265);
#4256=VERTEX_POINT('',#14269);
#4257=VERTEX_POINT('',#14270);
#4258=VERTEX_POINT('',#14272);
#4259=VERTEX_POINT('',#14274);
#4260=VERTEX_POINT('',#14278);
#4261=VERTEX_POINT('',#14280);
#4262=VERTEX_POINT('',#14287);
#4263=VERTEX_POINT('',#14289);
#4264=VERTEX_POINT('',#14296);
#4265=VERTEX_POINT('',#14298);
#4266=VERTEX_POINT('',#14305);
#4267=VERTEX_POINT('',#14307);
#4268=VERTEX_POINT('',#14314);
#4269=VERTEX_POINT('',#14316);
#4270=VERTEX_POINT('',#14323);
#4271=VERTEX_POINT('',#14325);
#4272=VERTEX_POINT('',#14332);
#4273=VERTEX_POINT('',#14334);
#4274=VERTEX_POINT('',#14341);
#4275=VERTEX_POINT('',#14343);
#4276=VERTEX_POINT('',#14350);
#4277=VERTEX_POINT('',#14352);
#4278=VERTEX_POINT('',#14359);
#4279=VERTEX_POINT('',#14361);
#4280=VERTEX_POINT('',#14368);
#4281=VERTEX_POINT('',#14370);
#4282=VERTEX_POINT('',#14377);
#4283=VERTEX_POINT('',#14379);
#4284=VERTEX_POINT('',#14386);
#4285=VERTEX_POINT('',#14388);
#4286=VERTEX_POINT('',#14395);
#4287=VERTEX_POINT('',#14397);
#4288=VERTEX_POINT('',#14404);
#4289=VERTEX_POINT('',#14406);
#4290=VERTEX_POINT('',#14413);
#4291=VERTEX_POINT('',#14415);
#4292=VERTEX_POINT('',#14422);
#4293=VERTEX_POINT('',#14424);
#4294=VERTEX_POINT('',#14431);
#4295=VERTEX_POINT('',#14433);
#4296=VERTEX_POINT('',#14440);
#4297=VERTEX_POINT('',#14442);
#4298=VERTEX_POINT('',#14449);
#4299=VERTEX_POINT('',#14451);
#4300=VERTEX_POINT('',#14458);
#4301=VERTEX_POINT('',#14460);
#4302=VERTEX_POINT('',#14467);
#4303=VERTEX_POINT('',#14469);
#4304=VERTEX_POINT('',#14476);
#4305=VERTEX_POINT('',#14478);
#4306=VERTEX_POINT('',#14485);
#4307=VERTEX_POINT('',#14487);
#4308=VERTEX_POINT('',#14494);
#4309=VERTEX_POINT('',#14496);
#4310=VERTEX_POINT('',#14503);
#4311=VERTEX_POINT('',#14505);
#4312=VERTEX_POINT('',#14512);
#4313=VERTEX_POINT('',#14514);
#4314=VERTEX_POINT('',#14521);
#4315=VERTEX_POINT('',#14523);
#4316=VERTEX_POINT('',#14530);
#4317=VERTEX_POINT('',#14532);
#4318=VERTEX_POINT('',#14539);
#4319=VERTEX_POINT('',#14541);
#4320=VERTEX_POINT('',#14548);
#4321=VERTEX_POINT('',#14550);
#4322=VERTEX_POINT('',#14557);
#4323=VERTEX_POINT('',#14559);
#4324=VERTEX_POINT('',#14566);
#4325=VERTEX_POINT('',#14568);
#4326=VERTEX_POINT('',#14575);
#4327=VERTEX_POINT('',#14577);
#4328=VERTEX_POINT('',#14584);
#4329=VERTEX_POINT('',#14586);
#4330=VERTEX_POINT('',#14593);
#4331=VERTEX_POINT('',#14595);
#4332=VERTEX_POINT('',#14602);
#4333=VERTEX_POINT('',#14604);
#4334=VERTEX_POINT('',#14611);
#4335=VERTEX_POINT('',#14613);
#4336=VERTEX_POINT('',#14620);
#4337=VERTEX_POINT('',#14622);
#4338=VERTEX_POINT('',#14629);
#4339=VERTEX_POINT('',#14631);
#4340=VERTEX_POINT('',#14638);
#4341=VERTEX_POINT('',#14639);
#4342=VERTEX_POINT('',#14674);
#4343=VERTEX_POINT('',#14676);
#4344=VERTEX_POINT('',#14713);
#4345=VERTEX_POINT('',#14714);
#4346=VERTEX_POINT('',#14719);
#4347=VERTEX_POINT('',#14799);
#4348=VERTEX_POINT('',#14864);
#4349=VERTEX_POINT('',#14871);
#4350=VERTEX_POINT('',#14872);
#4351=VERTEX_POINT('',#14874);
#4352=VERTEX_POINT('',#14879);
#4353=VERTEX_POINT('',#14968);
#4354=VERTEX_POINT('',#15037);
#4355=VERTEX_POINT('',#15040);
#4356=VERTEX_POINT('',#15042);
#4357=VERTEX_POINT('',#15044);
#4358=VERTEX_POINT('',#15299);
#4359=VERTEX_POINT('',#15502);
#4360=VERTEX_POINT('',#15802);
#4361=VERTEX_POINT('',#16162);
#4362=VERTEX_POINT('',#16230);
#4363=VERTEX_POINT('',#16470);
#4364=VERTEX_POINT('',#16535);
#4365=VERTEX_POINT('',#16671);
#4366=VERTEX_POINT('',#16986);
#4367=VERTEX_POINT('',#16989);
#4368=VERTEX_POINT('',#16991);
#4369=VERTEX_POINT('',#17021);
#4370=VERTEX_POINT('',#17024);
#4371=VERTEX_POINT('',#17025);
#4372=VERTEX_POINT('',#17325);
#4373=VERTEX_POINT('',#17326);
#4374=VERTEX_POINT('',#17627);
#4375=VERTEX_POINT('',#17635);
#4376=VERTEX_POINT('',#17636);
#4377=VERTEX_POINT('',#17638);
#4378=VERTEX_POINT('',#17640);
#4379=VERTEX_POINT('',#17644);
#4380=VERTEX_POINT('',#17646);
#4381=VERTEX_POINT('',#17650);
#4382=VERTEX_POINT('',#17654);
#4383=VERTEX_POINT('',#17663);
#4384=VERTEX_POINT('',#17664);
#4385=VERTEX_POINT('',#17668);
#4386=VERTEX_POINT('',#17670);
#4387=VERTEX_POINT('',#17674);
#4388=VERTEX_POINT('',#17678);
#4389=VERTEX_POINT('',#17682);
#4390=VERTEX_POINT('',#17686);
#4391=VERTEX_POINT('',#17690);
#4392=VERTEX_POINT('',#17694);
#4393=VERTEX_POINT('',#17698);
#4394=VERTEX_POINT('',#17702);
#4395=VERTEX_POINT('',#17704);
#4396=VERTEX_POINT('',#17710);
#4397=VERTEX_POINT('',#17714);
#4398=VERTEX_POINT('',#17718);
#4399=VERTEX_POINT('',#17722);
#4400=VERTEX_POINT('',#17725);
#4401=VERTEX_POINT('',#17733);
#4402=VERTEX_POINT('',#17735);
#4403=VERTEX_POINT('',#17737);
#4404=VERTEX_POINT('',#17739);
#4405=VERTEX_POINT('',#17742);
#4406=VERTEX_POINT('',#17744);
#4407=VERTEX_POINT('',#17748);
#4408=VERTEX_POINT('',#17750);
#4409=VERTEX_POINT('',#17753);
#4410=VERTEX_POINT('',#17754);
#4411=VERTEX_POINT('',#17759);
#4412=VERTEX_POINT('',#17762);
#4413=VERTEX_POINT('',#17766);
#4414=VERTEX_POINT('',#17768);
#4415=VERTEX_POINT('',#17771);
#4416=VERTEX_POINT('',#17773);
#4417=VERTEX_POINT('',#17776);
#4418=VERTEX_POINT('',#17781);
#4419=VERTEX_POINT('',#17786);
#4420=VERTEX_POINT('',#17790);
#4421=VERTEX_POINT('',#17792);
#4422=VERTEX_POINT('',#17794);
#4423=VERTEX_POINT('',#17796);
#4424=VERTEX_POINT('',#17799);
#4425=VERTEX_POINT('',#17801);
#4426=VERTEX_POINT('',#17808);
#4427=VERTEX_POINT('',#17816);
#4428=VERTEX_POINT('',#17821);
#4429=VERTEX_POINT('',#17826);
#4430=VERTEX_POINT('',#17836);
#4431=VERTEX_POINT('',#17837);
#4432=VERTEX_POINT('',#17839);
#4433=VERTEX_POINT('',#17841);
#4434=VERTEX_POINT('',#17845);
#4435=VERTEX_POINT('',#17846);
#4436=VERTEX_POINT('',#17848);
#4437=VERTEX_POINT('',#17850);
#4438=VERTEX_POINT('',#17854);
#4439=VERTEX_POINT('',#17856);
#4440=VERTEX_POINT('',#17860);
#4441=VERTEX_POINT('',#17862);
#4442=VERTEX_POINT('',#17866);
#4443=VERTEX_POINT('',#17868);
#4444=VERTEX_POINT('',#17870);
#4445=VERTEX_POINT('',#17872);
#4446=VERTEX_POINT('',#17874);
#4447=VERTEX_POINT('',#17876);
#4448=VERTEX_POINT('',#17878);
#4449=VERTEX_POINT('',#17881);
#4450=VERTEX_POINT('',#17883);
#4451=VERTEX_POINT('',#17885);
#4452=VERTEX_POINT('',#17887);
#4453=VERTEX_POINT('',#17889);
#4454=VERTEX_POINT('',#17891);
#4455=VERTEX_POINT('',#17893);
#4456=VERTEX_POINT('',#17896);
#4457=VERTEX_POINT('',#17899);
#4458=VERTEX_POINT('',#17901);
#4459=VERTEX_POINT('',#17903);
#4460=VERTEX_POINT('',#17905);
#4461=VERTEX_POINT('',#17907);
#4462=VERTEX_POINT('',#17909);
#4463=VERTEX_POINT('',#17911);
#4464=VERTEX_POINT('',#17914);
#4465=VERTEX_POINT('',#17916);
#4466=VERTEX_POINT('',#17918);
#4467=VERTEX_POINT('',#17920);
#4468=VERTEX_POINT('',#17922);
#4469=VERTEX_POINT('',#17924);
#4470=VERTEX_POINT('',#17926);
#4471=VERTEX_POINT('',#17929);
#4472=VERTEX_POINT('',#17932);
#4473=VERTEX_POINT('',#17933);
#4474=VERTEX_POINT('',#17935);
#4475=VERTEX_POINT('',#17975);
#4476=VERTEX_POINT('',#17976);
#4477=VERTEX_POINT('',#17979);
#4478=VERTEX_POINT('',#17983);
#4479=VERTEX_POINT('',#17986);
#4480=VERTEX_POINT('',#17994);
#4481=VERTEX_POINT('',#17997);
#4482=VERTEX_POINT('',#17998);
#4483=VERTEX_POINT('',#18000);
#4484=VERTEX_POINT('',#18004);
#4485=VERTEX_POINT('',#18005);
#4486=VERTEX_POINT('',#18043);
#4487=VERTEX_POINT('',#18046);
#4488=VERTEX_POINT('',#18047);
#4489=VERTEX_POINT('',#18049);
#4490=VERTEX_POINT('',#18054);
#4491=VERTEX_POINT('',#18055);
#4492=VERTEX_POINT('',#18057);
#4493=VERTEX_POINT('',#18059);
#4494=VERTEX_POINT('',#18061);
#4495=VERTEX_POINT('',#18063);
#4496=VERTEX_POINT('',#18065);
#4497=VERTEX_POINT('',#18067);
#4498=VERTEX_POINT('',#18071);
#4499=VERTEX_POINT('',#18072);
#4500=VERTEX_POINT('',#18077);
#4501=VERTEX_POINT('',#18079);
#4502=VERTEX_POINT('',#18083);
#4503=VERTEX_POINT('',#18085);
#4504=VERTEX_POINT('',#18089);
#4505=VERTEX_POINT('',#18091);
#4506=VERTEX_POINT('',#18100);
#4507=VERTEX_POINT('',#18405);
#4508=VERTEX_POINT('',#18406);
#4509=VERTEX_POINT('',#18408);
#4510=VERTEX_POINT('',#18422);
#4511=VERTEX_POINT('',#18484);
#4512=VERTEX_POINT('',#18851);
#4513=VERTEX_POINT('',#19220);
#4514=VERTEX_POINT('',#19222);
#4515=VERTEX_POINT('',#19886);
#4516=VERTEX_POINT('',#19887);
#4517=VERTEX_POINT('',#19889);
#4518=VERTEX_POINT('',#19903);
#4519=VERTEX_POINT('',#19965);
#4520=VERTEX_POINT('',#20332);
#4521=VERTEX_POINT('',#20701);
#4522=VERTEX_POINT('',#20703);
#4523=VERTEX_POINT('',#21076);
#4524=VERTEX_POINT('',#21077);
#4525=VERTEX_POINT('',#21089);
#4526=VERTEX_POINT('',#21095);
#4527=VERTEX_POINT('',#21097);
#4528=VERTEX_POINT('',#21099);
#4529=VERTEX_POINT('',#21118);
#4530=VERTEX_POINT('',#21120);
#4531=VERTEX_POINT('',#21137);
#4532=VERTEX_POINT('',#21140);
#4533=VERTEX_POINT('',#21159);
#4534=VERTEX_POINT('',#21177);
#4535=VERTEX_POINT('',#21178);
#4536=VERTEX_POINT('',#21209);
#4537=VERTEX_POINT('',#21211);
#4538=VERTEX_POINT('',#21243);
#4539=VERTEX_POINT('',#21244);
#4540=VERTEX_POINT('',#21275);
#4541=VERTEX_POINT('',#21277);
#4542=VERTEX_POINT('',#21309);
#4543=VERTEX_POINT('',#21310);
#4544=VERTEX_POINT('',#21341);
#4545=VERTEX_POINT('',#21343);
#4546=VERTEX_POINT('',#21375);
#4547=VERTEX_POINT('',#21376);
#4548=VERTEX_POINT('',#21407);
#4549=VERTEX_POINT('',#21409);
#4550=VERTEX_POINT('',#21441);
#4551=VERTEX_POINT('',#21442);
#4552=VERTEX_POINT('',#21473);
#4553=VERTEX_POINT('',#21475);
#4554=VERTEX_POINT('',#21507);
#4555=VERTEX_POINT('',#21508);
#4556=VERTEX_POINT('',#21539);
#4557=VERTEX_POINT('',#21541);
#4558=VERTEX_POINT('',#21573);
#4559=VERTEX_POINT('',#21574);
#4560=VERTEX_POINT('',#21605);
#4561=VERTEX_POINT('',#21607);
#4562=VERTEX_POINT('',#21639);
#4563=VERTEX_POINT('',#21640);
#4564=VERTEX_POINT('',#21671);
#4565=VERTEX_POINT('',#21673);
#4566=VERTEX_POINT('',#21705);
#4567=VERTEX_POINT('',#21706);
#4568=VERTEX_POINT('',#21737);
#4569=VERTEX_POINT('',#21739);
#4570=VERTEX_POINT('',#21772);
#4571=VERTEX_POINT('',#21774);
#4572=VERTEX_POINT('',#21776);
#4573=VERTEX_POINT('',#21787);
#4574=VERTEX_POINT('',#21798);
#4575=VERTEX_POINT('',#21801);
#4576=VERTEX_POINT('',#21822);
#4577=VERTEX_POINT('',#21823);
#4578=VERTEX_POINT('',#21861);
#4579=VERTEX_POINT('',#21862);
#4580=VERTEX_POINT('',#21865);
#4581=VERTEX_POINT('',#21867);
#4582=VERTEX_POINT('',#21891);
#4583=VERTEX_POINT('',#21894);
#4584=VERTEX_POINT('',#21919);
#4585=VERTEX_POINT('',#21960);
#4586=VERTEX_POINT('',#21962);
#4587=VERTEX_POINT('',#21965);
#4588=VERTEX_POINT('',#21967);
#4589=VERTEX_POINT('',#21970);
#4590=VERTEX_POINT('',#21971);
#4591=VERTEX_POINT('',#21973);
#4592=VERTEX_POINT('',#21975);
#4593=VERTEX_POINT('',#21986);
#4594=VERTEX_POINT('',#21997);
#4595=VERTEX_POINT('',#21999);
#4596=VERTEX_POINT('',#22010);
#4597=VERTEX_POINT('',#22021);
#4598=VERTEX_POINT('',#22024);
#4599=VERTEX_POINT('',#22045);
#4600=VERTEX_POINT('',#22067);
#4601=VERTEX_POINT('',#22068);
#4602=VERTEX_POINT('',#22106);
#4603=VERTEX_POINT('',#22107);
#4604=VERTEX_POINT('',#22150);
#4605=VERTEX_POINT('',#22151);
#4606=VERTEX_POINT('',#22207);
#4607=VERTEX_POINT('',#22209);
#4608=VERTEX_POINT('',#23777);
#4609=VERTEX_POINT('',#23779);
#4610=VERTEX_POINT('',#23781);
#4611=VERTEX_POINT('',#23792);
#4612=VERTEX_POINT('',#23803);
#4613=VERTEX_POINT('',#23806);
#4614=VERTEX_POINT('',#23827);
#4615=VERTEX_POINT('',#23828);
#4616=VERTEX_POINT('',#23866);
#4617=VERTEX_POINT('',#23869);
#4618=VERTEX_POINT('',#23872);
#4619=VERTEX_POINT('',#23877);
#4620=VERTEX_POINT('',#23885);
#4621=VERTEX_POINT('',#23887);
#4622=VERTEX_POINT('',#23890);
#4623=VERTEX_POINT('',#23894);
#4624=VERTEX_POINT('',#23896);
#4625=VERTEX_POINT('',#23899);
#4626=VERTEX_POINT('',#23904);
#4627=VERTEX_POINT('',#23908);
#4628=VERTEX_POINT('',#23912);
#4629=VERTEX_POINT('',#23913);
#4630=VERTEX_POINT('',#23915);
#4631=VERTEX_POINT('',#23917);
#4632=VERTEX_POINT('',#23919);
#4633=VERTEX_POINT('',#23921);
#4634=VERTEX_POINT('',#23925);
#4635=VERTEX_POINT('',#23926);
#4636=VERTEX_POINT('',#23931);
#4637=VERTEX_POINT('',#23935);
#4638=VERTEX_POINT('',#23939);
#4639=VERTEX_POINT('',#23943);
#4640=VERTEX_POINT('',#23951);
#4641=VERTEX_POINT('',#23952);
#4642=VERTEX_POINT('',#23956);
#4643=VERTEX_POINT('',#23957);
#4644=VERTEX_POINT('',#27730);
#4645=VERTEX_POINT('',#27731);
#4646=VERTEX_POINT('',#27734);
#4647=VERTEX_POINT('',#27738);
#4648=VERTEX_POINT('',#27741);
#4649=VERTEX_POINT('',#27743);
#4650=VERTEX_POINT('',#27746);
#4651=VERTEX_POINT('',#27750);
#4652=VERTEX_POINT('',#27751);
#4653=VERTEX_POINT('',#27753);
#4654=VERTEX_POINT('',#27755);
#4655=VERTEX_POINT('',#27759);
#4656=VERTEX_POINT('',#27761);
#4657=VERTEX_POINT('',#27765);
#4658=VERTEX_POINT('',#27769);
#4659=VERTEX_POINT('',#27780);
#4660=VERTEX_POINT('',#27781);
#4661=VERTEX_POINT('',#27783);
#4662=VERTEX_POINT('',#27785);
#4663=VERTEX_POINT('',#27788);
#4664=VERTEX_POINT('',#27789);
#4665=VERTEX_POINT('',#27791);
#4666=VERTEX_POINT('',#27793);
#4667=VERTEX_POINT('',#27795);
#4668=VERTEX_POINT('',#27797);
#4669=VERTEX_POINT('',#27799);
#4670=VERTEX_POINT('',#27801);
#4671=VERTEX_POINT('',#27803);
#4672=VERTEX_POINT('',#27805);
#4673=VERTEX_POINT('',#27807);
#4674=VERTEX_POINT('',#27809);
#4675=VERTEX_POINT('',#27813);
#4676=VERTEX_POINT('',#27814);
#4677=VERTEX_POINT('',#27819);
#4678=VERTEX_POINT('',#27823);
#4679=VERTEX_POINT('',#27829);
#4680=VERTEX_POINT('',#27830);
#4681=VERTEX_POINT('',#27832);
#4682=VERTEX_POINT('',#27834);
#4683=VERTEX_POINT('',#27836);
#4684=VERTEX_POINT('',#27838);
#4685=VERTEX_POINT('',#27840);
#4686=VERTEX_POINT('',#27842);
#4687=VERTEX_POINT('',#27844);
#4688=VERTEX_POINT('',#27846);
#4689=VERTEX_POINT('',#27848);
#4690=VERTEX_POINT('',#27850);
#4691=VERTEX_POINT('',#27854);
#4692=VERTEX_POINT('',#27856);
#4693=VERTEX_POINT('',#27860);
#4694=VERTEX_POINT('',#27864);
#4695=VERTEX_POINT('',#27868);
#4696=VERTEX_POINT('',#27872);
#4697=VERTEX_POINT('',#27876);
#4698=VERTEX_POINT('',#27880);
#4699=VERTEX_POINT('',#27884);
#4700=VERTEX_POINT('',#27888);
#4701=VERTEX_POINT('',#27892);
#4702=VERTEX_POINT('',#27896);
#4703=VERTEX_POINT('',#27903);
#4704=VERTEX_POINT('',#27905);
#4705=VERTEX_POINT('',#27909);
#4706=VERTEX_POINT('',#27913);
#4707=VERTEX_POINT('',#27917);
#4708=VERTEX_POINT('',#27921);
#4709=VERTEX_POINT('',#27925);
#4710=VERTEX_POINT('',#27929);
#4711=VERTEX_POINT('',#27933);
#4712=VERTEX_POINT('',#27937);
#4713=VERTEX_POINT('',#27941);
#4714=VERTEX_POINT('',#27945);
#4715=VERTEX_POINT('',#27953);
#4716=VERTEX_POINT('',#27955);
#4717=VERTEX_POINT('',#27962);
#4718=VERTEX_POINT('',#27964);
#4719=VERTEX_POINT('',#27971);
#4720=VERTEX_POINT('',#27973);
#4721=VERTEX_POINT('',#27976);
#4722=VERTEX_POINT('',#27978);
#4723=VERTEX_POINT('',#28000);
#4724=VERTEX_POINT('',#28002);
#4725=VERTEX_POINT('',#28006);
#4726=VERTEX_POINT('',#28009);
#4727=VERTEX_POINT('',#28014);
#4728=VERTEX_POINT('',#28016);
#4729=VERTEX_POINT('',#28019);
#4730=VERTEX_POINT('',#28024);
#4731=VERTEX_POINT('',#28031);
#4732=VERTEX_POINT('',#28032);
#4733=VERTEX_POINT('',#28034);
#4734=VERTEX_POINT('',#28043);
#4735=VERTEX_POINT('',#28045);
#4736=VERTEX_POINT('',#28052);
#4737=VERTEX_POINT('',#28054);
#4738=VERTEX_POINT('',#28061);
#4739=VERTEX_POINT('',#28070);
#4740=VERTEX_POINT('',#28071);
#4741=VERTEX_POINT('',#28073);
#4742=VERTEX_POINT('',#28080);
#4743=VERTEX_POINT('',#28082);
#4744=VERTEX_POINT('',#28091);
#4745=VERTEX_POINT('',#28093);
#4746=VERTEX_POINT('',#28100);
#4747=VERTEX_POINT('',#28109);
#4748=VERTEX_POINT('',#28110);
#4749=VERTEX_POINT('',#28112);
#4750=VERTEX_POINT('',#28119);
#4751=VERTEX_POINT('',#28121);
#4752=VERTEX_POINT('',#28130);
#4753=VERTEX_POINT('',#28132);
#4754=VERTEX_POINT('',#28139);
#4755=VERTEX_POINT('',#28148);
#4756=VERTEX_POINT('',#28149);
#4757=VERTEX_POINT('',#28151);
#4758=VERTEX_POINT('',#28158);
#4759=VERTEX_POINT('',#28160);
#4760=VERTEX_POINT('',#28169);
#4761=VERTEX_POINT('',#28171);
#4762=VERTEX_POINT('',#28178);
#4763=VERTEX_POINT('',#28180);
#4764=VERTEX_POINT('',#28189);
#4765=VERTEX_POINT('',#28190);
#4766=VERTEX_POINT('',#28192);
#4767=VERTEX_POINT('',#28201);
#4768=VERTEX_POINT('',#28203);
#4769=VERTEX_POINT('',#28210);
#4770=VERTEX_POINT('',#28212);
#4771=VERTEX_POINT('',#28219);
#4772=VERTEX_POINT('',#28228);
#4773=VERTEX_POINT('',#28229);
#4774=VERTEX_POINT('',#28231);
#4775=VERTEX_POINT('',#28238);
#4776=VERTEX_POINT('',#28240);
#4777=VERTEX_POINT('',#28249);
#4778=VERTEX_POINT('',#28251);
#4779=VERTEX_POINT('',#28258);
#4780=VERTEX_POINT('',#28267);
#4781=VERTEX_POINT('',#28268);
#4782=VERTEX_POINT('',#28270);
#4783=VERTEX_POINT('',#28277);
#4784=VERTEX_POINT('',#28279);
#4785=VERTEX_POINT('',#28288);
#4786=VERTEX_POINT('',#28290);
#4787=VERTEX_POINT('',#28297);
#4788=VERTEX_POINT('',#28306);
#4789=VERTEX_POINT('',#28307);
#4790=VERTEX_POINT('',#28309);
#4791=VERTEX_POINT('',#28316);
#4792=VERTEX_POINT('',#28318);
#4793=VERTEX_POINT('',#28327);
#4794=VERTEX_POINT('',#28329);
#4795=VERTEX_POINT('',#28336);
#4796=VERTEX_POINT('',#28345);
#4797=VERTEX_POINT('',#28346);
#4798=VERTEX_POINT('',#28348);
#4799=VERTEX_POINT('',#28355);
#4800=VERTEX_POINT('',#28357);
#4801=VERTEX_POINT('',#28366);
#4802=VERTEX_POINT('',#28368);
#4803=VERTEX_POINT('',#28375);
#4804=VERTEX_POINT('',#28391);
#4805=VERTEX_POINT('',#28393);
#4806=VERTEX_POINT('',#28397);
#4807=VERTEX_POINT('',#28400);
#4808=VERTEX_POINT('',#28402);
#4809=VERTEX_POINT('',#28406);
#4810=VERTEX_POINT('',#28408);
#4811=VERTEX_POINT('',#28412);
#4812=VERTEX_POINT('',#28413);
#4813=VERTEX_POINT('',#28421);
#4814=VERTEX_POINT('',#28430);
#4815=VERTEX_POINT('',#28432);
#4816=VERTEX_POINT('',#28439);
#4817=VERTEX_POINT('',#28448);
#4818=VERTEX_POINT('',#28450);
#4819=VERTEX_POINT('',#28453);
#4820=VERTEX_POINT('',#28454);
#4821=VERTEX_POINT('',#28459);
#4822=VERTEX_POINT('',#28462);
#4823=VERTEX_POINT('',#28463);
#4824=VERTEX_POINT('',#28500);
#4825=VERTEX_POINT('',#28501);
#4826=VERTEX_POINT('',#28538);
#4827=VERTEX_POINT('',#28539);
#4828=VERTEX_POINT('',#28576);
#4829=VERTEX_POINT('',#28577);
#4830=VERTEX_POINT('',#28614);
#4831=VERTEX_POINT('',#28615);
#4832=VERTEX_POINT('',#28654);
#4833=VERTEX_POINT('',#28657);
#4834=VERTEX_POINT('',#28659);
#4835=VERTEX_POINT('',#29257);
#4836=VERTEX_POINT('',#29261);
#4837=VERTEX_POINT('',#29262);
#4838=VERTEX_POINT('',#29299);
#4839=VERTEX_POINT('',#29300);
#4840=VERTEX_POINT('',#29337);
#4841=VERTEX_POINT('',#29338);
#4842=VERTEX_POINT('',#29375);
#4843=VERTEX_POINT('',#29376);
#4844=VERTEX_POINT('',#29413);
#4845=VERTEX_POINT('',#29414);
#4846=VERTEX_POINT('',#29463);
#4847=VERTEX_POINT('',#29469);
#4848=VERTEX_POINT('',#29472);
#4849=VERTEX_POINT('',#29477);
#4850=VERTEX_POINT('',#29478);
#4851=VERTEX_POINT('',#29480);
#4852=VERTEX_POINT('',#29482);
#4853=VERTEX_POINT('',#29503);
#4854=VERTEX_POINT('',#29504);
#4855=VERTEX_POINT('',#29506);
#4856=VERTEX_POINT('',#29508);
#4857=VERTEX_POINT('',#29593);
#4858=VERTEX_POINT('',#29594);
#4859=VERTEX_POINT('',#29596);
#4860=VERTEX_POINT('',#29598);
#4861=VERTEX_POINT('',#29619);
#4862=VERTEX_POINT('',#29620);
#4863=VERTEX_POINT('',#29622);
#4864=VERTEX_POINT('',#29624);
#4865=VERTEX_POINT('',#29712);
#4866=VERTEX_POINT('',#29713);
#4867=VERTEX_POINT('',#29715);
#4868=VERTEX_POINT('',#29717);
#4869=VERTEX_POINT('',#29802);
#4870=VERTEX_POINT('',#29803);
#4871=VERTEX_POINT('',#29822);
#4872=VERTEX_POINT('',#29824);
#4873=VERTEX_POINT('',#29828);
#4874=VERTEX_POINT('',#29829);
#4875=VERTEX_POINT('',#29831);
#4876=VERTEX_POINT('',#29833);
#4877=VERTEX_POINT('',#29918);
#4878=VERTEX_POINT('',#29919);
#4879=VERTEX_POINT('',#29921);
#4880=VERTEX_POINT('',#29923);
#4881=VERTEX_POINT('',#29944);
#4882=VERTEX_POINT('',#29945);
#4883=VERTEX_POINT('',#29947);
#4884=VERTEX_POINT('',#29949);
#4885=VERTEX_POINT('',#30037);
#4886=VERTEX_POINT('',#30038);
#4887=VERTEX_POINT('',#30040);
#4888=VERTEX_POINT('',#30042);
#4889=VERTEX_POINT('',#31160);
#4890=VERTEX_POINT('',#31162);
#4891=VERTEX_POINT('',#31165);
#4892=VERTEX_POINT('',#31167);
#4893=VERTEX_POINT('',#31168);
#4894=VERTEX_POINT('',#31170);
#4895=VERTEX_POINT('',#31172);
#4896=VERTEX_POINT('',#31174);
#4897=VERTEX_POINT('',#31176);
#4898=VERTEX_POINT('',#31178);
#4899=VERTEX_POINT('',#31180);
#4900=VERTEX_POINT('',#31182);
#4901=VERTEX_POINT('',#31184);
#4902=VERTEX_POINT('',#31186);
#4903=VERTEX_POINT('',#31188);
#4904=VERTEX_POINT('',#31190);
#4905=VERTEX_POINT('',#31192);
#4906=VERTEX_POINT('',#31194);
#4907=VERTEX_POINT('',#31196);
#4908=VERTEX_POINT('',#31198);
#4909=VERTEX_POINT('',#31200);
#4910=VERTEX_POINT('',#31202);
#4911=VERTEX_POINT('',#31204);
#4912=VERTEX_POINT('',#31206);
#4913=VERTEX_POINT('',#31208);
#4914=VERTEX_POINT('',#31210);
#4915=VERTEX_POINT('',#31212);
#4916=VERTEX_POINT('',#31216);
#4917=VERTEX_POINT('',#31217);
#4918=VERTEX_POINT('',#31222);
#4919=VERTEX_POINT('',#31223);
#4920=VERTEX_POINT('',#31228);
#4921=VERTEX_POINT('',#31229);
#4922=VERTEX_POINT('',#31234);
#4923=VERTEX_POINT('',#31236);
#4924=VERTEX_POINT('',#31240);
#4925=VERTEX_POINT('',#31244);
#4926=VERTEX_POINT('',#31245);
#4927=VERTEX_POINT('',#31250);
#4928=VERTEX_POINT('',#31251);
#4929=VERTEX_POINT('',#31256);
#4930=VERTEX_POINT('',#31257);
#4931=VERTEX_POINT('',#31260);
#4932=VERTEX_POINT('',#31264);
#4933=VERTEX_POINT('',#31265);
#4934=VERTEX_POINT('',#31267);
#4935=VERTEX_POINT('',#31270);
#4936=VERTEX_POINT('',#31272);
#4937=VERTEX_POINT('',#31275);
#4938=VERTEX_POINT('',#31277);
#4939=VERTEX_POINT('',#31280);
#4940=VERTEX_POINT('',#31282);
#4941=VERTEX_POINT('',#31285);
#4942=VERTEX_POINT('',#31287);
#4943=VERTEX_POINT('',#31290);
#4944=VERTEX_POINT('',#31292);
#4945=VERTEX_POINT('',#31295);
#4946=VERTEX_POINT('',#31595);
#4947=VERTEX_POINT('',#31596);
#4948=VERTEX_POINT('',#31598);
#4949=VERTEX_POINT('',#31616);
#4950=VERTEX_POINT('',#31666);
#4951=VERTEX_POINT('',#31993);
#4952=VERTEX_POINT('',#32322);
#4953=VERTEX_POINT('',#32324);
#4954=VERTEX_POINT('',#32657);
#4955=VERTEX_POINT('',#32659);
#4956=VERTEX_POINT('',#32662);
#4957=VERTEX_POINT('',#32666);
#4958=VERTEX_POINT('',#32670);
#4959=VERTEX_POINT('',#32674);
#4960=VERTEX_POINT('',#32677);
#4961=VERTEX_POINT('',#32681);
#4962=VERTEX_POINT('',#32684);
#4963=VERTEX_POINT('',#32686);
#4964=VERTEX_POINT('',#32690);
#4965=VERTEX_POINT('',#32691);
#4966=VERTEX_POINT('',#32696);
#4967=VERTEX_POINT('',#32698);
#4968=VERTEX_POINT('',#32702);
#4969=VERTEX_POINT('',#32703);
#4970=VERTEX_POINT('',#32708);
#4971=VERTEX_POINT('',#32712);
#4972=VERTEX_POINT('',#32718);
#4973=VERTEX_POINT('',#32719);
#4974=VERTEX_POINT('',#32732);
#4975=VERTEX_POINT('',#32735);
#4976=VERTEX_POINT('',#32739);
#4977=VERTEX_POINT('',#32740);
#4978=VERTEX_POINT('',#32745);
#4979=VERTEX_POINT('',#32747);
#4980=VERTEX_POINT('',#32750);
#4981=VERTEX_POINT('',#32751);
#4982=VERTEX_POINT('',#32758);
#4983=VERTEX_POINT('',#32762);
#4984=VERTEX_POINT('',#32765);
#4985=VERTEX_POINT('',#32769);
#4986=VERTEX_POINT('',#32775);
#4987=VERTEX_POINT('',#32780);
#4988=VERTEX_POINT('',#32781);
#4989=VERTEX_POINT('',#32783);
#4990=VERTEX_POINT('',#32785);
#4991=VERTEX_POINT('',#32787);
#4992=VERTEX_POINT('',#32789);
#4993=VERTEX_POINT('',#32791);
#4994=VERTEX_POINT('',#32793);
#4995=VERTEX_POINT('',#32795);
#4996=VERTEX_POINT('',#32797);
#4997=VERTEX_POINT('',#32799);
#4998=VERTEX_POINT('',#32801);
#4999=VERTEX_POINT('',#32804);
#5000=VERTEX_POINT('',#32807);
#5001=VERTEX_POINT('',#32808);
#5002=VERTEX_POINT('',#32810);
#5003=VERTEX_POINT('',#32812);
#5004=VERTEX_POINT('',#32814);
#5005=VERTEX_POINT('',#32816);
#5006=VERTEX_POINT('',#32818);
#5007=VERTEX_POINT('',#32820);
#5008=VERTEX_POINT('',#32822);
#5009=VERTEX_POINT('',#32824);
#5010=VERTEX_POINT('',#32826);
#5011=VERTEX_POINT('',#32828);
#5012=VERTEX_POINT('',#32831);
#5013=VERTEX_POINT('',#32834);
#5014=VERTEX_POINT('',#32835);
#5015=VERTEX_POINT('',#32840);
#5016=VERTEX_POINT('',#32844);
#5017=VERTEX_POINT('',#32856);
#5018=VERTEX_POINT('',#32860);
#5019=VERTEX_POINT('',#32872);
#5020=VERTEX_POINT('',#32876);
#5021=VERTEX_POINT('',#32888);
#5022=VERTEX_POINT('',#32892);
#5023=VERTEX_POINT('',#32904);
#5024=VERTEX_POINT('',#32908);
#5025=EDGE_CURVE('',#4100,#4101,#2600,.T.);
#5026=EDGE_CURVE('',#4101,#4102,#2212,.T.);
#5027=EDGE_CURVE('',#4103,#4102,#2601,.T.);
#5028=EDGE_CURVE('',#4103,#4100,#2213,.T.);
#5029=EDGE_CURVE('',#4104,#4105,#2602,.T.);
#5030=EDGE_CURVE('',#4105,#4106,#2214,.T.);
#5031=EDGE_CURVE('',#4107,#4106,#2603,.T.);
#5032=EDGE_CURVE('',#4107,#4104,#2215,.T.);
#5033=EDGE_CURVE('',#4108,#4109,#2604,.T.);
#5034=EDGE_CURVE('',#4109,#4110,#2216,.T.);
#5035=EDGE_CURVE('',#4111,#4110,#2605,.T.);
#5036=EDGE_CURVE('',#4111,#4108,#2217,.T.);
#5037=EDGE_CURVE('',#4112,#4113,#2606,.T.);
#5038=EDGE_CURVE('',#4113,#4114,#2218,.T.);
#5039=EDGE_CURVE('',#4115,#4114,#2607,.T.);
#5040=EDGE_CURVE('',#4115,#4112,#2219,.T.);
#5041=EDGE_CURVE('',#4116,#4117,#2608,.T.);
#5042=EDGE_CURVE('',#4117,#4118,#2220,.T.);
#5043=EDGE_CURVE('',#4119,#4118,#2609,.T.);
#5044=EDGE_CURVE('',#4119,#4116,#2221,.T.);
#5045=EDGE_CURVE('',#4120,#4121,#2610,.T.);
#5046=EDGE_CURVE('',#4121,#4122,#2222,.T.);
#5047=EDGE_CURVE('',#4123,#4122,#2611,.T.);
#5048=EDGE_CURVE('',#4123,#4120,#2223,.T.);
#5049=EDGE_CURVE('',#4124,#4125,#2612,.T.);
#5050=EDGE_CURVE('',#4125,#4126,#2224,.T.);
#5051=EDGE_CURVE('',#4127,#4126,#2613,.T.);
#5052=EDGE_CURVE('',#4127,#4124,#2225,.T.);
#5053=EDGE_CURVE('',#4128,#4129,#2614,.T.);
#5054=EDGE_CURVE('',#4129,#4130,#2226,.T.);
#5055=EDGE_CURVE('',#4131,#4130,#2615,.T.);
#5056=EDGE_CURVE('',#4131,#4128,#2227,.T.);
#5057=EDGE_CURVE('',#4132,#4133,#2616,.T.);
#5058=EDGE_CURVE('',#4133,#4134,#2228,.T.);
#5059=EDGE_CURVE('',#4135,#4134,#2617,.T.);
#5060=EDGE_CURVE('',#4135,#4132,#2229,.T.);
#5061=EDGE_CURVE('',#4136,#4137,#2618,.T.);
#5062=EDGE_CURVE('',#4137,#4138,#2230,.T.);
#5063=EDGE_CURVE('',#4139,#4138,#2619,.T.);
#5064=EDGE_CURVE('',#4139,#4136,#2231,.T.);
#5065=EDGE_CURVE('',#4140,#4141,#2620,.T.);
#5066=EDGE_CURVE('',#4141,#4142,#2232,.T.);
#5067=EDGE_CURVE('',#4143,#4142,#2621,.T.);
#5068=EDGE_CURVE('',#4143,#4140,#2233,.T.);
#5069=EDGE_CURVE('',#4144,#4145,#2622,.T.);
#5070=EDGE_CURVE('',#4145,#4146,#2234,.T.);
#5071=EDGE_CURVE('',#4147,#4146,#2623,.T.);
#5072=EDGE_CURVE('',#4147,#4144,#2235,.T.);
#5073=EDGE_CURVE('',#4148,#4149,#2624,.T.);
#5074=EDGE_CURVE('',#4149,#4150,#2236,.T.);
#5075=EDGE_CURVE('',#4151,#4150,#2625,.T.);
#5076=EDGE_CURVE('',#4151,#4148,#2237,.T.);
#5077=EDGE_CURVE('',#4152,#4153,#2626,.T.);
#5078=EDGE_CURVE('',#4153,#4154,#2238,.T.);
#5079=EDGE_CURVE('',#4155,#4154,#2627,.T.);
#5080=EDGE_CURVE('',#4155,#4152,#2239,.T.);
#5081=EDGE_CURVE('',#4156,#4157,#2628,.T.);
#5082=EDGE_CURVE('',#4157,#4158,#2240,.T.);
#5083=EDGE_CURVE('',#4159,#4158,#2629,.T.);
#5084=EDGE_CURVE('',#4159,#4156,#2241,.T.);
#5085=EDGE_CURVE('',#4160,#4161,#2630,.T.);
#5086=EDGE_CURVE('',#4161,#4162,#2242,.T.);
#5087=EDGE_CURVE('',#4163,#4162,#2631,.T.);
#5088=EDGE_CURVE('',#4163,#4160,#2243,.T.);
#5089=EDGE_CURVE('',#4164,#4165,#2632,.T.);
#5090=EDGE_CURVE('',#4165,#4166,#2244,.T.);
#5091=EDGE_CURVE('',#4167,#4166,#2633,.T.);
#5092=EDGE_CURVE('',#4167,#4164,#2245,.T.);
#5093=EDGE_CURVE('',#4168,#4169,#2634,.T.);
#5094=EDGE_CURVE('',#4169,#4170,#2246,.T.);
#5095=EDGE_CURVE('',#4171,#4170,#2635,.T.);
#5096=EDGE_CURVE('',#4171,#4168,#2247,.T.);
#5097=EDGE_CURVE('',#4172,#4173,#2636,.T.);
#5098=EDGE_CURVE('',#4173,#4174,#2248,.T.);
#5099=EDGE_CURVE('',#4175,#4174,#2637,.T.);
#5100=EDGE_CURVE('',#4175,#4172,#2249,.T.);
#5101=EDGE_CURVE('',#4176,#4177,#2638,.T.);
#5102=EDGE_CURVE('',#4177,#4178,#2250,.T.);
#5103=EDGE_CURVE('',#4179,#4178,#2639,.T.);
#5104=EDGE_CURVE('',#4179,#4176,#2251,.T.);
#5105=EDGE_CURVE('',#4180,#4181,#2640,.T.);
#5106=EDGE_CURVE('',#4181,#4182,#2252,.T.);
#5107=EDGE_CURVE('',#4183,#4182,#2641,.T.);
#5108=EDGE_CURVE('',#4183,#4180,#2253,.T.);
#5109=EDGE_CURVE('',#4184,#4185,#2642,.T.);
#5110=EDGE_CURVE('',#4185,#4186,#2254,.T.);
#5111=EDGE_CURVE('',#4187,#4186,#2643,.T.);
#5112=EDGE_CURVE('',#4187,#4184,#2255,.T.);
#5113=EDGE_CURVE('',#4188,#4189,#2644,.T.);
#5114=EDGE_CURVE('',#4189,#4190,#2256,.T.);
#5115=EDGE_CURVE('',#4191,#4190,#2645,.T.);
#5116=EDGE_CURVE('',#4191,#4188,#2257,.T.);
#5117=EDGE_CURVE('',#4192,#4193,#2646,.T.);
#5118=EDGE_CURVE('',#4193,#4194,#2258,.T.);
#5119=EDGE_CURVE('',#4195,#4194,#2647,.T.);
#5120=EDGE_CURVE('',#4195,#4192,#2259,.T.);
#5121=EDGE_CURVE('',#4196,#4197,#2648,.T.);
#5122=EDGE_CURVE('',#4197,#4198,#2260,.T.);
#5123=EDGE_CURVE('',#4199,#4198,#2649,.T.);
#5124=EDGE_CURVE('',#4199,#4196,#2261,.T.);
#5125=EDGE_CURVE('',#4200,#4201,#2650,.T.);
#5126=EDGE_CURVE('',#4201,#4202,#2262,.T.);
#5127=EDGE_CURVE('',#4203,#4202,#2651,.T.);
#5128=EDGE_CURVE('',#4203,#4200,#2263,.T.);
#5129=EDGE_CURVE('',#4204,#4205,#2652,.T.);
#5130=EDGE_CURVE('',#4205,#4206,#2264,.T.);
#5131=EDGE_CURVE('',#4207,#4206,#2653,.T.);
#5132=EDGE_CURVE('',#4207,#4204,#2265,.T.);
#5133=EDGE_CURVE('',#4208,#4209,#2654,.T.);
#5134=EDGE_CURVE('',#4209,#4210,#2266,.T.);
#5135=EDGE_CURVE('',#4211,#4210,#2655,.T.);
#5136=EDGE_CURVE('',#4211,#4208,#2267,.T.);
#5137=EDGE_CURVE('',#4212,#4213,#2656,.T.);
#5138=EDGE_CURVE('',#4213,#4214,#2268,.T.);
#5139=EDGE_CURVE('',#4215,#4214,#2657,.T.);
#5140=EDGE_CURVE('',#4215,#4212,#2269,.T.);
#5141=EDGE_CURVE('',#4216,#4217,#2658,.T.);
#5142=EDGE_CURVE('',#4217,#4218,#2270,.T.);
#5143=EDGE_CURVE('',#4219,#4218,#2659,.T.);
#5144=EDGE_CURVE('',#4219,#4216,#2271,.T.);
#5145=EDGE_CURVE('',#4220,#4221,#2660,.T.);
#5146=EDGE_CURVE('',#4221,#4222,#2272,.T.);
#5147=EDGE_CURVE('',#4223,#4222,#2661,.T.);
#5148=EDGE_CURVE('',#4223,#4220,#2273,.T.);
#5149=EDGE_CURVE('',#4224,#4225,#2662,.T.);
#5150=EDGE_CURVE('',#4225,#4226,#2274,.T.);
#5151=EDGE_CURVE('',#4227,#4226,#2663,.T.);
#5152=EDGE_CURVE('',#4227,#4224,#2275,.T.);
#5153=EDGE_CURVE('',#4228,#4229,#2664,.T.);
#5154=EDGE_CURVE('',#4229,#4230,#2276,.T.);
#5155=EDGE_CURVE('',#4231,#4230,#2665,.T.);
#5156=EDGE_CURVE('',#4231,#4228,#2277,.T.);
#5157=EDGE_CURVE('',#4232,#4233,#2666,.T.);
#5158=EDGE_CURVE('',#4233,#4234,#2278,.T.);
#5159=EDGE_CURVE('',#4235,#4234,#2667,.T.);
#5160=EDGE_CURVE('',#4235,#4232,#2279,.T.);
#5161=EDGE_CURVE('',#4236,#4237,#2668,.T.);
#5162=EDGE_CURVE('',#4237,#4238,#2280,.T.);
#5163=EDGE_CURVE('',#4239,#4238,#2669,.T.);
#5164=EDGE_CURVE('',#4239,#4236,#2281,.T.);
#5165=EDGE_CURVE('',#4240,#4241,#2670,.T.);
#5166=EDGE_CURVE('',#4241,#4242,#2282,.T.);
#5167=EDGE_CURVE('',#4243,#4242,#2671,.T.);
#5168=EDGE_CURVE('',#4243,#4240,#2283,.T.);
#5169=EDGE_CURVE('',#4244,#4245,#2672,.T.);
#5170=EDGE_CURVE('',#4245,#4246,#2284,.T.);
#5171=EDGE_CURVE('',#4247,#4246,#2673,.T.);
#5172=EDGE_CURVE('',#4247,#4244,#2285,.T.);
#5173=EDGE_CURVE('',#4248,#4249,#2674,.T.);
#5174=EDGE_CURVE('',#4249,#4250,#2286,.T.);
#5175=EDGE_CURVE('',#4251,#4250,#2675,.T.);
#5176=EDGE_CURVE('',#4251,#4248,#2287,.T.);
#5177=EDGE_CURVE('',#4252,#4253,#2676,.T.);
#5178=EDGE_CURVE('',#4253,#4254,#2288,.T.);
#5179=EDGE_CURVE('',#4255,#4254,#2677,.T.);
#5180=EDGE_CURVE('',#4255,#4252,#2289,.T.);
#5181=EDGE_CURVE('',#4256,#4257,#2678,.T.);
#5182=EDGE_CURVE('',#4257,#4258,#2290,.T.);
#5183=EDGE_CURVE('',#4259,#4258,#2679,.T.);
#5184=EDGE_CURVE('',#4259,#4256,#2291,.T.);
#5185=EDGE_CURVE('',#4260,#4254,#2680,.T.);
#5186=EDGE_CURVE('',#4261,#4260,#2681,.T.);
#5187=EDGE_CURVE('',#4261,#4255,#2682,.T.);
#5188=EDGE_CURVE('',#4257,#4260,#2683,.T.);
#5189=EDGE_CURVE('',#4256,#4261,#2684,.T.);
#5190=EDGE_CURVE('',#4262,#4250,#2685,.T.);
#5191=EDGE_CURVE('',#4263,#4262,#2686,.T.);
#5192=EDGE_CURVE('',#4263,#4251,#2687,.T.);
#5193=EDGE_CURVE('',#4253,#4262,#2688,.T.);
#5194=EDGE_CURVE('',#4252,#4263,#2689,.T.);
#5195=EDGE_CURVE('',#4264,#4246,#2690,.T.);
#5196=EDGE_CURVE('',#4265,#4264,#2691,.T.);
#5197=EDGE_CURVE('',#4265,#4247,#2692,.T.);
#5198=EDGE_CURVE('',#4249,#4264,#2693,.T.);
#5199=EDGE_CURVE('',#4248,#4265,#2694,.T.);
#5200=EDGE_CURVE('',#4266,#4242,#2695,.T.);
#5201=EDGE_CURVE('',#4267,#4266,#2696,.T.);
#5202=EDGE_CURVE('',#4267,#4243,#2697,.T.);
#5203=EDGE_CURVE('',#4245,#4266,#2698,.T.);
#5204=EDGE_CURVE('',#4244,#4267,#2699,.T.);
#5205=EDGE_CURVE('',#4268,#4238,#2700,.T.);
#5206=EDGE_CURVE('',#4269,#4268,#2701,.T.);
#5207=EDGE_CURVE('',#4269,#4239,#2702,.T.);
#5208=EDGE_CURVE('',#4241,#4268,#2703,.T.);
#5209=EDGE_CURVE('',#4240,#4269,#2704,.T.);
#5210=EDGE_CURVE('',#4270,#4234,#2705,.T.);
#5211=EDGE_CURVE('',#4271,#4270,#2706,.T.);
#5212=EDGE_CURVE('',#4271,#4235,#2707,.T.);
#5213=EDGE_CURVE('',#4237,#4270,#2708,.T.);
#5214=EDGE_CURVE('',#4236,#4271,#2709,.T.);
#5215=EDGE_CURVE('',#4272,#4230,#2710,.T.);
#5216=EDGE_CURVE('',#4273,#4272,#2711,.T.);
#5217=EDGE_CURVE('',#4273,#4231,#2712,.T.);
#5218=EDGE_CURVE('',#4233,#4272,#2713,.T.);
#5219=EDGE_CURVE('',#4232,#4273,#2714,.T.);
#5220=EDGE_CURVE('',#4274,#4226,#2715,.T.);
#5221=EDGE_CURVE('',#4275,#4274,#2716,.T.);
#5222=EDGE_CURVE('',#4275,#4227,#2717,.T.);
#5223=EDGE_CURVE('',#4229,#4274,#2718,.T.);
#5224=EDGE_CURVE('',#4228,#4275,#2719,.T.);
#5225=EDGE_CURVE('',#4276,#4222,#2720,.T.);
#5226=EDGE_CURVE('',#4277,#4276,#2721,.T.);
#5227=EDGE_CURVE('',#4277,#4223,#2722,.T.);
#5228=EDGE_CURVE('',#4225,#4276,#2723,.T.);
#5229=EDGE_CURVE('',#4224,#4277,#2724,.T.);
#5230=EDGE_CURVE('',#4278,#4218,#2725,.T.);
#5231=EDGE_CURVE('',#4279,#4278,#2726,.T.);
#5232=EDGE_CURVE('',#4279,#4219,#2727,.T.);
#5233=EDGE_CURVE('',#4221,#4278,#2728,.T.);
#5234=EDGE_CURVE('',#4220,#4279,#2729,.T.);
#5235=EDGE_CURVE('',#4280,#4214,#2730,.T.);
#5236=EDGE_CURVE('',#4281,#4280,#2731,.T.);
#5237=EDGE_CURVE('',#4281,#4215,#2732,.T.);
#5238=EDGE_CURVE('',#4217,#4280,#2733,.T.);
#5239=EDGE_CURVE('',#4216,#4281,#2734,.T.);
#5240=EDGE_CURVE('',#4282,#4210,#2735,.T.);
#5241=EDGE_CURVE('',#4283,#4282,#2736,.T.);
#5242=EDGE_CURVE('',#4283,#4211,#2737,.T.);
#5243=EDGE_CURVE('',#4213,#4282,#2738,.T.);
#5244=EDGE_CURVE('',#4212,#4283,#2739,.T.);
#5245=EDGE_CURVE('',#4284,#4206,#2740,.T.);
#5246=EDGE_CURVE('',#4285,#4284,#2741,.T.);
#5247=EDGE_CURVE('',#4285,#4207,#2742,.T.);
#5248=EDGE_CURVE('',#4209,#4284,#2743,.T.);
#5249=EDGE_CURVE('',#4208,#4285,#2744,.T.);
#5250=EDGE_CURVE('',#4286,#4202,#2745,.T.);
#5251=EDGE_CURVE('',#4287,#4286,#2746,.T.);
#5252=EDGE_CURVE('',#4287,#4203,#2747,.T.);
#5253=EDGE_CURVE('',#4205,#4286,#2748,.T.);
#5254=EDGE_CURVE('',#4204,#4287,#2749,.T.);
#5255=EDGE_CURVE('',#4288,#4198,#2750,.T.);
#5256=EDGE_CURVE('',#4289,#4288,#2751,.T.);
#5257=EDGE_CURVE('',#4289,#4199,#2752,.T.);
#5258=EDGE_CURVE('',#4201,#4288,#2753,.T.);
#5259=EDGE_CURVE('',#4200,#4289,#2754,.T.);
#5260=EDGE_CURVE('',#4290,#4194,#2755,.T.);
#5261=EDGE_CURVE('',#4291,#4290,#2756,.T.);
#5262=EDGE_CURVE('',#4291,#4195,#2757,.T.);
#5263=EDGE_CURVE('',#4197,#4290,#2758,.T.);
#5264=EDGE_CURVE('',#4196,#4291,#2759,.T.);
#5265=EDGE_CURVE('',#4292,#4190,#2760,.T.);
#5266=EDGE_CURVE('',#4293,#4292,#2761,.T.);
#5267=EDGE_CURVE('',#4293,#4191,#2762,.T.);
#5268=EDGE_CURVE('',#4193,#4292,#2763,.T.);
#5269=EDGE_CURVE('',#4192,#4293,#2764,.T.);
#5270=EDGE_CURVE('',#4294,#4186,#2765,.T.);
#5271=EDGE_CURVE('',#4295,#4294,#2766,.T.);
#5272=EDGE_CURVE('',#4295,#4187,#2767,.T.);
#5273=EDGE_CURVE('',#4189,#4294,#2768,.T.);
#5274=EDGE_CURVE('',#4188,#4295,#2769,.T.);
#5275=EDGE_CURVE('',#4296,#4182,#2770,.T.);
#5276=EDGE_CURVE('',#4297,#4296,#2771,.T.);
#5277=EDGE_CURVE('',#4297,#4183,#2772,.T.);
#5278=EDGE_CURVE('',#4185,#4296,#2773,.T.);
#5279=EDGE_CURVE('',#4184,#4297,#2774,.T.);
#5280=EDGE_CURVE('',#4298,#4178,#2775,.T.);
#5281=EDGE_CURVE('',#4299,#4298,#2776,.T.);
#5282=EDGE_CURVE('',#4299,#4179,#2777,.T.);
#5283=EDGE_CURVE('',#4181,#4298,#2778,.T.);
#5284=EDGE_CURVE('',#4180,#4299,#2779,.T.);
#5285=EDGE_CURVE('',#4300,#4174,#2780,.T.);
#5286=EDGE_CURVE('',#4301,#4300,#2781,.T.);
#5287=EDGE_CURVE('',#4301,#4175,#2782,.T.);
#5288=EDGE_CURVE('',#4177,#4300,#2783,.T.);
#5289=EDGE_CURVE('',#4176,#4301,#2784,.T.);
#5290=EDGE_CURVE('',#4302,#4170,#2785,.T.);
#5291=EDGE_CURVE('',#4303,#4302,#2786,.T.);
#5292=EDGE_CURVE('',#4303,#4171,#2787,.T.);
#5293=EDGE_CURVE('',#4173,#4302,#2788,.T.);
#5294=EDGE_CURVE('',#4172,#4303,#2789,.T.);
#5295=EDGE_CURVE('',#4304,#4166,#2790,.T.);
#5296=EDGE_CURVE('',#4305,#4304,#2791,.T.);
#5297=EDGE_CURVE('',#4305,#4167,#2792,.T.);
#5298=EDGE_CURVE('',#4169,#4304,#2793,.T.);
#5299=EDGE_CURVE('',#4168,#4305,#2794,.T.);
#5300=EDGE_CURVE('',#4306,#4162,#2795,.T.);
#5301=EDGE_CURVE('',#4307,#4306,#2796,.T.);
#5302=EDGE_CURVE('',#4307,#4163,#2797,.T.);
#5303=EDGE_CURVE('',#4165,#4306,#2798,.T.);
#5304=EDGE_CURVE('',#4164,#4307,#2799,.T.);
#5305=EDGE_CURVE('',#4308,#4158,#2800,.T.);
#5306=EDGE_CURVE('',#4309,#4308,#2801,.T.);
#5307=EDGE_CURVE('',#4309,#4159,#2802,.T.);
#5308=EDGE_CURVE('',#4161,#4308,#2803,.T.);
#5309=EDGE_CURVE('',#4160,#4309,#2804,.T.);
#5310=EDGE_CURVE('',#4310,#4154,#2805,.T.);
#5311=EDGE_CURVE('',#4311,#4310,#2806,.T.);
#5312=EDGE_CURVE('',#4311,#4155,#2807,.T.);
#5313=EDGE_CURVE('',#4157,#4310,#2808,.T.);
#5314=EDGE_CURVE('',#4156,#4311,#2809,.T.);
#5315=EDGE_CURVE('',#4312,#4150,#2810,.T.);
#5316=EDGE_CURVE('',#4313,#4312,#2811,.T.);
#5317=EDGE_CURVE('',#4313,#4151,#2812,.T.);
#5318=EDGE_CURVE('',#4153,#4312,#2813,.T.);
#5319=EDGE_CURVE('',#4152,#4313,#2814,.T.);
#5320=EDGE_CURVE('',#4314,#4146,#2815,.T.);
#5321=EDGE_CURVE('',#4315,#4314,#2816,.T.);
#5322=EDGE_CURVE('',#4315,#4147,#2817,.T.);
#5323=EDGE_CURVE('',#4149,#4314,#2818,.T.);
#5324=EDGE_CURVE('',#4148,#4315,#2819,.T.);
#5325=EDGE_CURVE('',#4316,#4142,#2820,.T.);
#5326=EDGE_CURVE('',#4317,#4316,#2821,.T.);
#5327=EDGE_CURVE('',#4317,#4143,#2822,.T.);
#5328=EDGE_CURVE('',#4145,#4316,#2823,.T.);
#5329=EDGE_CURVE('',#4144,#4317,#2824,.T.);
#5330=EDGE_CURVE('',#4318,#4138,#2825,.T.);
#5331=EDGE_CURVE('',#4319,#4318,#2826,.T.);
#5332=EDGE_CURVE('',#4319,#4139,#2827,.T.);
#5333=EDGE_CURVE('',#4141,#4318,#2828,.T.);
#5334=EDGE_CURVE('',#4140,#4319,#2829,.T.);
#5335=EDGE_CURVE('',#4320,#4134,#2830,.T.);
#5336=EDGE_CURVE('',#4321,#4320,#2831,.T.);
#5337=EDGE_CURVE('',#4321,#4135,#2832,.T.);
#5338=EDGE_CURVE('',#4137,#4320,#2833,.T.);
#5339=EDGE_CURVE('',#4136,#4321,#2834,.T.);
#5340=EDGE_CURVE('',#4322,#4130,#2835,.T.);
#5341=EDGE_CURVE('',#4323,#4322,#2836,.T.);
#5342=EDGE_CURVE('',#4323,#4131,#2837,.T.);
#5343=EDGE_CURVE('',#4133,#4322,#2838,.T.);
#5344=EDGE_CURVE('',#4132,#4323,#2839,.T.);
#5345=EDGE_CURVE('',#4324,#4126,#2840,.T.);
#5346=EDGE_CURVE('',#4325,#4324,#2841,.T.);
#5347=EDGE_CURVE('',#4325,#4127,#2842,.T.);
#5348=EDGE_CURVE('',#4129,#4324,#2843,.T.);
#5349=EDGE_CURVE('',#4128,#4325,#2844,.T.);
#5350=EDGE_CURVE('',#4326,#4122,#2845,.T.);
#5351=EDGE_CURVE('',#4327,#4326,#2846,.T.);
#5352=EDGE_CURVE('',#4327,#4123,#2847,.T.);
#5353=EDGE_CURVE('',#4125,#4326,#2848,.T.);
#5354=EDGE_CURVE('',#4124,#4327,#2849,.T.);
#5355=EDGE_CURVE('',#4328,#4118,#2850,.T.);
#5356=EDGE_CURVE('',#4329,#4328,#2851,.T.);
#5357=EDGE_CURVE('',#4329,#4119,#2852,.T.);
#5358=EDGE_CURVE('',#4121,#4328,#2853,.T.);
#5359=EDGE_CURVE('',#4120,#4329,#2854,.T.);
#5360=EDGE_CURVE('',#4330,#4114,#2855,.T.);
#5361=EDGE_CURVE('',#4331,#4330,#2856,.T.);
#5362=EDGE_CURVE('',#4331,#4115,#2857,.T.);
#5363=EDGE_CURVE('',#4117,#4330,#2858,.T.);
#5364=EDGE_CURVE('',#4116,#4331,#2859,.T.);
#5365=EDGE_CURVE('',#4332,#4110,#2860,.T.);
#5366=EDGE_CURVE('',#4333,#4332,#2861,.T.);
#5367=EDGE_CURVE('',#4333,#4111,#2862,.T.);
#5368=EDGE_CURVE('',#4113,#4332,#2863,.T.);
#5369=EDGE_CURVE('',#4112,#4333,#2864,.T.);
#5370=EDGE_CURVE('',#4334,#4106,#2865,.T.);
#5371=EDGE_CURVE('',#4335,#4334,#2866,.T.);
#5372=EDGE_CURVE('',#4335,#4107,#2867,.T.);
#5373=EDGE_CURVE('',#4109,#4334,#2868,.T.);
#5374=EDGE_CURVE('',#4108,#4335,#2869,.T.);
#5375=EDGE_CURVE('',#4336,#4102,#2870,.T.);
#5376=EDGE_CURVE('',#4337,#4336,#2871,.T.);
#5377=EDGE_CURVE('',#4337,#4103,#2872,.T.);
#5378=EDGE_CURVE('',#4105,#4336,#2873,.T.);
#5379=EDGE_CURVE('',#4104,#4337,#2874,.T.);
#5380=EDGE_CURVE('',#4338,#4258,#2875,.T.);
#5381=EDGE_CURVE('',#4339,#4338,#2876,.T.);
#5382=EDGE_CURVE('',#4339,#4259,#2877,.T.);
#5383=EDGE_CURVE('',#4101,#4338,#2878,.T.);
#5384=EDGE_CURVE('',#4100,#4339,#2879,.T.);
#5385=EDGE_CURVE('',#4340,#4341,#554,.T.);
#5386=EDGE_CURVE('',#4341,#4342,#2292,.T.);
#5387=EDGE_CURVE('',#4342,#4343,#555,.T.);
#5388=EDGE_CURVE('',#4343,#4340,#2293,.T.);
#5389=EDGE_CURVE('',#4344,#4345,#556,.T.);
#5390=EDGE_CURVE('',#4345,#4346,#557,.T.);
#5391=EDGE_CURVE('',#4346,#4347,#558,.T.);
#5392=EDGE_CURVE('',#4347,#4348,#559,.T.);
#5393=EDGE_CURVE('',#4348,#4344,#2294,.T.);
#5394=EDGE_CURVE('',#4349,#4350,#2295,.T.);
#5395=EDGE_CURVE('',#4350,#4351,#560,.T.);
#5396=EDGE_CURVE('',#4351,#4352,#561,.T.);
#5397=EDGE_CURVE('',#4352,#4353,#562,.T.);
#5398=EDGE_CURVE('',#4353,#4349,#563,.T.);
#5399=EDGE_CURVE('',#4354,#4354,#2296,.T.);
#5400=EDGE_CURVE('',#4355,#4355,#2297,.T.);
#5401=EDGE_CURVE('',#4355,#4356,#2880,.T.);
#5402=EDGE_CURVE('',#4356,#4357,#564,.T.);
#5403=EDGE_CURVE('',#4357,#4352,#565,.T.);
#5404=EDGE_CURVE('',#4352,#4358,#566,.T.);
#5405=EDGE_CURVE('',#4358,#4359,#567,.T.);
#5406=EDGE_CURVE('',#4359,#4346,#568,.T.);
#5407=EDGE_CURVE('',#4346,#4360,#569,.T.);
#5408=EDGE_CURVE('',#4360,#4356,#570,.T.);
#5409=EDGE_CURVE('',#4361,#4359,#2298,.T.);
#5410=EDGE_CURVE('',#4361,#4346,#571,.T.);
#5411=EDGE_CURVE('',#4362,#4358,#2299,.T.);
#5412=EDGE_CURVE('',#4362,#4341,#406,.T.);
#5413=EDGE_CURVE('',#4340,#4361,#407,.T.);
#5414=EDGE_CURVE('',#4352,#4362,#572,.T.);
#5415=EDGE_CURVE('',#4346,#4363,#573,.T.);
#5416=EDGE_CURVE('',#4360,#4363,#2300,.T.);
#5417=EDGE_CURVE('',#4363,#4343,#408,.T.);
#5418=EDGE_CURVE('',#4342,#4364,#409,.T.);
#5419=EDGE_CURVE('',#4357,#4364,#2301,.T.);
#5420=EDGE_CURVE('',#4364,#4352,#574,.T.);
#5421=EDGE_CURVE('',#4365,#4365,#2302,.T.);
#5422=EDGE_CURVE('',#4365,#4354,#2881,.T.);
#5423=EDGE_CURVE('',#4353,#4364,#2303,.T.);
#5424=EDGE_CURVE('',#4349,#4342,#2304,.T.);
#5425=EDGE_CURVE('',#4350,#4341,#2305,.T.);
#5426=EDGE_CURVE('',#4351,#4362,#2306,.T.);
#5427=EDGE_CURVE('',#4363,#4345,#2307,.T.);
#5428=EDGE_CURVE('',#4343,#4344,#2308,.T.);
#5429=EDGE_CURVE('',#4340,#4348,#2309,.T.);
#5430=EDGE_CURVE('',#4361,#4347,#2310,.T.);
#5431=EDGE_CURVE('',#4366,#4366,#2311,.T.);
#5432=EDGE_CURVE('',#4367,#4367,#2312,.T.);
#5433=EDGE_CURVE('',#4367,#4368,#2882,.T.);
#5434=EDGE_CURVE('',#4368,#4368,#2313,.T.);
#5435=EDGE_CURVE('',#4368,#4369,#2314,.T.);
#5436=EDGE_CURVE('',#4369,#4369,#2315,.T.);
#5437=EDGE_CURVE('',#4370,#4371,#575,.T.);
#5438=EDGE_CURVE('',#4371,#4370,#576,.T.);
#5439=EDGE_CURVE('',#4372,#4373,#577,.T.);
#5440=EDGE_CURVE('',#4373,#4372,#578,.T.);
#5441=EDGE_CURVE('',#4369,#4374,#2883,.T.);
#5442=EDGE_CURVE('',#4374,#4374,#2316,.T.);
#5443=EDGE_CURVE('',#4366,#4367,#2317,.T.);
#5444=EDGE_CURVE('',#4371,#4373,#2884,.T.);
#5445=EDGE_CURVE('',#4375,#4376,#2885,.T.);
#5446=EDGE_CURVE('',#4377,#4375,#2886,.T.);
#5447=EDGE_CURVE('',#4378,#4377,#2887,.T.);
#5448=EDGE_CURVE('',#4376,#4378,#2888,.T.);
#5449=EDGE_CURVE('',#4379,#4375,#2889,.T.);
#5450=EDGE_CURVE('',#4380,#4379,#2890,.T.);
#5451=EDGE_CURVE('',#4380,#4377,#2891,.T.);
#5452=EDGE_CURVE('',#4381,#4380,#2892,.T.);
#5453=EDGE_CURVE('',#4381,#4378,#2893,.T.);
#5454=EDGE_CURVE('',#4382,#4381,#2894,.T.);
#5455=EDGE_CURVE('',#4382,#4376,#2895,.T.);
#5456=EDGE_CURVE('',#4379,#4382,#2896,.T.);
#5457=EDGE_CURVE('',#4383,#4384,#181,.T.);
#5458=EDGE_CURVE('',#4383,#4385,#2897,.T.);
#5459=EDGE_CURVE('',#4385,#4386,#2898,.T.);
#5460=EDGE_CURVE('',#4384,#4386,#2899,.T.);
#5461=EDGE_CURVE('',#4384,#4387,#182,.T.);
#5462=EDGE_CURVE('',#4386,#4388,#2900,.T.);
#5463=EDGE_CURVE('',#4387,#4388,#2901,.T.);
#5464=EDGE_CURVE('',#4387,#4389,#183,.T.);
#5465=EDGE_CURVE('',#4388,#4390,#2902,.T.);
#5466=EDGE_CURVE('',#4389,#4390,#2903,.T.);
#5467=EDGE_CURVE('',#4389,#4391,#184,.T.);
#5468=EDGE_CURVE('',#4390,#4392,#2904,.T.);
#5469=EDGE_CURVE('',#4391,#4392,#2905,.T.);
#5470=EDGE_CURVE('',#4391,#4393,#185,.T.);
#5471=EDGE_CURVE('',#4392,#4394,#2906,.T.);
#5472=EDGE_CURVE('',#4395,#4394,#2907,.T.);
#5473=EDGE_CURVE('',#4393,#4395,#186,.T.);
#5474=EDGE_CURVE('',#4395,#4396,#187,.T.);
#5475=EDGE_CURVE('',#4394,#4397,#2908,.T.);
#5476=EDGE_CURVE('',#4396,#4397,#2909,.T.);
#5477=EDGE_CURVE('',#4396,#4398,#188,.T.);
#5478=EDGE_CURVE('',#4397,#4399,#2910,.T.);
#5479=EDGE_CURVE('',#4398,#4399,#2911,.T.);
#5480=EDGE_CURVE('',#4400,#4400,#2318,.T.);
#5481=EDGE_CURVE('',#4398,#4383,#189,.T.);
#5482=EDGE_CURVE('',#4399,#4385,#2912,.T.);
#5483=EDGE_CURVE('',#4401,#4401,#2319,.T.);
#5484=EDGE_CURVE('',#4401,#4402,#2913,.T.);
#5485=EDGE_CURVE('',#4403,#4402,#2914,.T.);
#5486=EDGE_CURVE('',#4403,#4404,#2915,.T.);
#5487=EDGE_CURVE('',#4404,#4404,#2320,.T.);
#5488=EDGE_CURVE('',#4405,#4403,#2321,.T.);
#5489=EDGE_CURVE('',#4406,#4405,#2916,.T.);
#5490=EDGE_CURVE('',#4402,#4406,#2322,.T.);
#5491=EDGE_CURVE('',#4407,#4407,#2323,.T.);
#5492=EDGE_CURVE('',#4408,#4408,#2324,.T.);
#5493=EDGE_CURVE('',#4409,#4410,#2325,.T.);
#5494=EDGE_CURVE('',#4410,#4407,#2917,.T.);
#5495=EDGE_CURVE('',#4410,#4409,#2326,.T.);
#5496=EDGE_CURVE('',#4411,#4411,#2327,.T.);
#5497=EDGE_CURVE('',#4412,#4412,#2328,.T.);
#5498=EDGE_CURVE('',#4412,#4408,#2918,.T.);
#5499=EDGE_CURVE('',#4413,#4413,#2329,.T.);
#5500=EDGE_CURVE('',#4414,#4414,#2330,.T.);
#5501=EDGE_CURVE('',#4415,#4415,#2331,.T.);
#5502=EDGE_CURVE('',#4416,#4416,#2332,.T.);
#5503=EDGE_CURVE('',#4417,#4417,#2333,.T.);
#5504=EDGE_CURVE('',#4417,#4416,#2919,.T.);
#5505=EDGE_CURVE('',#4418,#4418,#2334,.T.);
#5506=EDGE_CURVE('',#4418,#4415,#2920,.T.);
#5507=EDGE_CURVE('',#4419,#4419,#2335,.T.);
#5508=EDGE_CURVE('',#4419,#4414,#2921,.T.);
#5509=EDGE_CURVE('',#4420,#4420,#2336,.T.);
#5510=EDGE_CURVE('',#4420,#4421,#2922,.T.);
#5511=EDGE_CURVE('',#4421,#4422,#2923,.T.);
#5512=EDGE_CURVE('',#4422,#4423,#2924,.T.);
#5513=EDGE_CURVE('',#4423,#4423,#2337,.T.);
#5514=EDGE_CURVE('',#4422,#4424,#2338,.T.);
#5515=EDGE_CURVE('',#4424,#4425,#2925,.T.);
#5516=EDGE_CURVE('',#4425,#4421,#2339,.T.);
#5517=EDGE_CURVE('',#4406,#4421,#2926,.T.);
#5518=EDGE_CURVE('',#4425,#4402,#2927,.T.);
#5519=EDGE_CURVE('',#4426,#4426,#2340,.T.);
#5520=EDGE_CURVE('',#4424,#4403,#2928,.T.);
#5521=EDGE_CURVE('',#4405,#4422,#2929,.T.);
#5522=EDGE_CURVE('',#4427,#4427,#2341,.T.);
#5523=EDGE_CURVE('',#4427,#4426,#2930,.T.);
#5524=EDGE_CURVE('',#4428,#4428,#2342,.T.);
#5525=EDGE_CURVE('',#4428,#4400,#2931,.T.);
#5526=EDGE_CURVE('',#4393,#4429,#2932,.T.);
#5527=EDGE_CURVE('',#4429,#4429,#2343,.T.);
#5528=EDGE_CURVE('',#4409,#4411,#2933,.T.);
#5529=EDGE_CURVE('',#4423,#4413,#2934,.T.);
#5530=EDGE_CURVE('',#4430,#4431,#2935,.T.);
#5531=EDGE_CURVE('',#4431,#4432,#2344,.T.);
#5532=EDGE_CURVE('',#4433,#4432,#2936,.T.);
#5533=EDGE_CURVE('',#4430,#4433,#2345,.T.);
#5534=EDGE_CURVE('',#4434,#4435,#2346,.T.);
#5535=EDGE_CURVE('',#4436,#4434,#2937,.T.);
#5536=EDGE_CURVE('',#4436,#4437,#2347,.T.);
#5537=EDGE_CURVE('',#4437,#4435,#2938,.T.);
#5538=EDGE_CURVE('',#4434,#4438,#2939,.T.);
#5539=EDGE_CURVE('',#4439,#4438,#2940,.T.);
#5540=EDGE_CURVE('',#4436,#4439,#2941,.T.);
#5541=EDGE_CURVE('',#4440,#4435,#2942,.T.);
#5542=EDGE_CURVE('',#4441,#4437,#2943,.T.);
#5543=EDGE_CURVE('',#4441,#4440,#2944,.T.);
#5544=EDGE_CURVE('',#4439,#4442,#2945,.T.);
#5545=EDGE_CURVE('',#4442,#4443,#2946,.T.);
#5546=EDGE_CURVE('',#4443,#4444,#2947,.T.);
#5547=EDGE_CURVE('',#4444,#4445,#2948,.T.);
#5548=EDGE_CURVE('',#4445,#4446,#2949,.T.);
#5549=EDGE_CURVE('',#4446,#4447,#2950,.T.);
#5550=EDGE_CURVE('',#4447,#4448,#2951,.T.);
#5551=EDGE_CURVE('',#4448,#4430,#2952,.T.);
#5552=EDGE_CURVE('',#4449,#4433,#2953,.T.);
#5553=EDGE_CURVE('',#4450,#4449,#2954,.T.);
#5554=EDGE_CURVE('',#4451,#4450,#2955,.T.);
#5555=EDGE_CURVE('',#4452,#4451,#2956,.T.);
#5556=EDGE_CURVE('',#4453,#4452,#2957,.T.);
#5557=EDGE_CURVE('',#4454,#4453,#2958,.T.);
#5558=EDGE_CURVE('',#4455,#4454,#2959,.T.);
#5559=EDGE_CURVE('',#4441,#4455,#2960,.T.);
#5560=EDGE_CURVE('',#4456,#4456,#2348,.T.);
#5561=EDGE_CURVE('',#4440,#4457,#2961,.T.);
#5562=EDGE_CURVE('',#4457,#4458,#2962,.T.);
#5563=EDGE_CURVE('',#4458,#4459,#2963,.T.);
#5564=EDGE_CURVE('',#4459,#4460,#2964,.T.);
#5565=EDGE_CURVE('',#4460,#4461,#2965,.T.);
#5566=EDGE_CURVE('',#4461,#4462,#2966,.T.);
#5567=EDGE_CURVE('',#4462,#4463,#2967,.T.);
#5568=EDGE_CURVE('',#4463,#4432,#2968,.T.);
#5569=EDGE_CURVE('',#4464,#4431,#2969,.T.);
#5570=EDGE_CURVE('',#4465,#4464,#2970,.T.);
#5571=EDGE_CURVE('',#4466,#4465,#2971,.T.);
#5572=EDGE_CURVE('',#4467,#4466,#2972,.T.);
#5573=EDGE_CURVE('',#4468,#4467,#2973,.T.);
#5574=EDGE_CURVE('',#4469,#4468,#2974,.T.);
#5575=EDGE_CURVE('',#4470,#4469,#2975,.T.);
#5576=EDGE_CURVE('',#4438,#4470,#2976,.T.);
#5577=EDGE_CURVE('',#4471,#4471,#2349,.T.);
#5578=EDGE_CURVE('',#4472,#4473,#2350,.T.);
#5579=EDGE_CURVE('',#4473,#4474,#2977,.T.);
#5580=EDGE_CURVE('',#4474,#4474,#2351,.T.);
#5581=EDGE_CURVE('',#4473,#4472,#2352,.T.);
#5582=EDGE_CURVE('',#4455,#4457,#2978,.T.);
#5583=EDGE_CURVE('',#4454,#4458,#2979,.T.);
#5584=EDGE_CURVE('',#4453,#4459,#2980,.T.);
#5585=EDGE_CURVE('',#4452,#4460,#2981,.T.);
#5586=EDGE_CURVE('',#4451,#4461,#2982,.T.);
#5587=EDGE_CURVE('',#4450,#4462,#2983,.T.);
#5588=EDGE_CURVE('',#4449,#4463,#2984,.T.);
#5589=EDGE_CURVE('',#4442,#4470,#2985,.T.);
#5590=EDGE_CURVE('',#4443,#4469,#2986,.T.);
#5591=EDGE_CURVE('',#4444,#4468,#2987,.T.);
#5592=EDGE_CURVE('',#4445,#4467,#2988,.T.);
#5593=EDGE_CURVE('',#4446,#4466,#2989,.T.);
#5594=EDGE_CURVE('',#4447,#4465,#2990,.T.);
#5595=EDGE_CURVE('',#4448,#4464,#2991,.T.);
#5596=EDGE_CURVE('',#4472,#4471,#2992,.T.);
#5597=EDGE_CURVE('',#4474,#4456,#2993,.T.);
#5598=EDGE_CURVE('',#4475,#4476,#2353,.T.);
#5599=EDGE_CURVE('',#4476,#4475,#2354,.T.);
#5600=EDGE_CURVE('',#4475,#4477,#2994,.T.);
#5601=EDGE_CURVE('',#4477,#4477,#2355,.T.);
#5602=EDGE_CURVE('',#4478,#4478,#2356,.T.);
#5603=EDGE_CURVE('',#4479,#4479,#2357,.T.);
#5604=EDGE_CURVE('',#4476,#4479,#2995,.T.);
#5605=EDGE_CURVE('',#4477,#4478,#2996,.T.);
#5606=EDGE_CURVE('',#4480,#4480,#2358,.T.);
#5607=EDGE_CURVE('',#4481,#4482,#2359,.T.);
#5608=EDGE_CURVE('',#4482,#4483,#2997,.T.);
#5609=EDGE_CURVE('',#4483,#4483,#2360,.T.);
#5610=EDGE_CURVE('',#4482,#4481,#2361,.T.);
#5611=EDGE_CURVE('',#4484,#4485,#579,.T.);
#5612=EDGE_CURVE('',#4485,#4484,#580,.T.);
#5613=EDGE_CURVE('',#4486,#4486,#2362,.T.);
#5614=EDGE_CURVE('',#4487,#4488,#2363,.T.);
#5615=EDGE_CURVE('',#4488,#4489,#2998,.T.);
#5616=EDGE_CURVE('',#4489,#4489,#2364,.T.);
#5617=EDGE_CURVE('',#4488,#4487,#2365,.T.);
#5618=EDGE_CURVE('',#4490,#4491,#2366,.T.);
#5619=EDGE_CURVE('',#4490,#4492,#2367,.T.);
#5620=EDGE_CURVE('',#4493,#4492,#2999,.T.);
#5621=EDGE_CURVE('',#4493,#4494,#2368,.T.);
#5622=EDGE_CURVE('',#4495,#4494,#2369,.T.);
#5623=EDGE_CURVE('',#4495,#4496,#2370,.T.);
#5624=EDGE_CURVE('',#4497,#4496,#3000,.T.);
#5625=EDGE_CURVE('',#4497,#4491,#2371,.T.);
#5626=EDGE_CURVE('',#4498,#4499,#2372,.T.);
#5627=EDGE_CURVE('',#4498,#4490,#3001,.T.);
#5628=EDGE_CURVE('',#4491,#4499,#3002,.T.);
#5629=EDGE_CURVE('',#4496,#4500,#3003,.T.);
#5630=EDGE_CURVE('',#4501,#4500,#3004,.T.);
#5631=EDGE_CURVE('',#4501,#4497,#3005,.T.);
#5632=EDGE_CURVE('',#4494,#4502,#3006,.T.);
#5633=EDGE_CURVE('',#4503,#4502,#2373,.T.);
#5634=EDGE_CURVE('',#4503,#4495,#3007,.T.);
#5635=EDGE_CURVE('',#4492,#4504,#3008,.T.);
#5636=EDGE_CURVE('',#4505,#4504,#3009,.T.);
#5637=EDGE_CURVE('',#4505,#4493,#3010,.T.);
#5638=EDGE_CURVE('',#4504,#4498,#2374,.T.);
#5639=EDGE_CURVE('',#4499,#4501,#2375,.T.);
#5640=EDGE_CURVE('',#4500,#4503,#2376,.T.);
#5641=EDGE_CURVE('',#4502,#4505,#2377,.T.);
#5642=EDGE_CURVE('',#4506,#4506,#2378,.T.);
#5643=EDGE_CURVE('',#4506,#4485,#3011,.T.);
#5644=EDGE_CURVE('',#4481,#4480,#3012,.T.);
#5645=EDGE_CURVE('',#4487,#4486,#3013,.T.);
#5646=EDGE_CURVE('',#4507,#4508,#2379,.T.);
#5647=EDGE_CURVE('',#4509,#4508,#190,.T.);
#5648=EDGE_CURVE('',#4510,#4509,#191,.T.);
#5649=EDGE_CURVE('',#4511,#4510,#2380,.T.);
#5650=EDGE_CURVE('',#4511,#4507,#192,.T.);
#5651=EDGE_CURVE('',#4512,#4511,#2381,.T.);
#5652=EDGE_CURVE('',#4512,#4510,#193,.T.);
#5653=EDGE_CURVE('',#4510,#4509,#194,.T.);
#5654=EDGE_CURVE('',#4509,#4507,#2382,.T.);
#5655=EDGE_CURVE('',#4513,#4512,#2383,.T.);
#5656=EDGE_CURVE('',#4513,#4514,#195,.T.);
#5657=EDGE_CURVE('',#4514,#4509,#2384,.T.);
#5658=EDGE_CURVE('',#4510,#4513,#2385,.T.);
#5659=EDGE_CURVE('',#4508,#4514,#2386,.T.);
#5660=EDGE_CURVE('',#4515,#4516,#2387,.T.);
#5661=EDGE_CURVE('',#4517,#4516,#196,.T.);
#5662=EDGE_CURVE('',#4518,#4517,#197,.T.);
#5663=EDGE_CURVE('',#4519,#4518,#2388,.T.);
#5664=EDGE_CURVE('',#4519,#4515,#198,.T.);
#5665=EDGE_CURVE('',#4520,#4519,#2389,.T.);
#5666=EDGE_CURVE('',#4520,#4518,#199,.T.);
#5667=EDGE_CURVE('',#4518,#4517,#200,.T.);
#5668=EDGE_CURVE('',#4517,#4515,#2390,.T.);
#5669=EDGE_CURVE('',#4521,#4520,#2391,.T.);
#5670=EDGE_CURVE('',#4521,#4522,#201,.T.);
#5671=EDGE_CURVE('',#4522,#4517,#2392,.T.);
#5672=EDGE_CURVE('',#4518,#4521,#2393,.T.);
#5673=EDGE_CURVE('',#4516,#4522,#2394,.T.);
#5674=EDGE_CURVE('',#4523,#4524,#2395,.T.);
#5675=EDGE_CURVE('',#4525,#4525,#2396,.T.);
#5676=EDGE_CURVE('',#4525,#4525,#2397,.T.);
#5677=EDGE_CURVE('',#4526,#4526,#2398,.T.);
#5678=EDGE_CURVE('',#4526,#4527,#3014,.T.);
#5679=EDGE_CURVE('',#4528,#4527,#581,.T.);
#5680=EDGE_CURVE('',#4529,#4528,#3015,.T.);
#5681=EDGE_CURVE('',#4530,#4529,#582,.T.);
#5682=EDGE_CURVE('',#4530,#4531,#3016,.T.);
#5683=EDGE_CURVE('',#4531,#4531,#2399,.T.);
#5684=EDGE_CURVE('',#4532,#4530,#583,.T.);
#5685=EDGE_CURVE('',#4533,#4532,#3017,.T.);
#5686=EDGE_CURVE('',#4527,#4533,#584,.T.);
#5687=EDGE_CURVE('',#4534,#4535,#585,.T.);
#5688=EDGE_CURVE('',#4536,#4534,#3018,.T.);
#5689=EDGE_CURVE('',#4537,#4536,#586,.T.);
#5690=EDGE_CURVE('',#4535,#4537,#3019,.T.);
#5691=EDGE_CURVE('',#4538,#4539,#587,.T.);
#5692=EDGE_CURVE('',#4540,#4538,#3020,.T.);
#5693=EDGE_CURVE('',#4541,#4540,#588,.T.);
#5694=EDGE_CURVE('',#4539,#4541,#3021,.T.);
#5695=EDGE_CURVE('',#4542,#4543,#589,.T.);
#5696=EDGE_CURVE('',#4544,#4542,#3022,.T.);
#5697=EDGE_CURVE('',#4545,#4544,#590,.T.);
#5698=EDGE_CURVE('',#4543,#4545,#3023,.T.);
#5699=EDGE_CURVE('',#4546,#4547,#591,.T.);
#5700=EDGE_CURVE('',#4548,#4546,#3024,.T.);
#5701=EDGE_CURVE('',#4549,#4548,#592,.T.);
#5702=EDGE_CURVE('',#4547,#4549,#3025,.T.);
#5703=EDGE_CURVE('',#4550,#4551,#593,.T.);
#5704=EDGE_CURVE('',#4552,#4550,#3026,.T.);
#5705=EDGE_CURVE('',#4553,#4552,#594,.T.);
#5706=EDGE_CURVE('',#4551,#4553,#3027,.T.);
#5707=EDGE_CURVE('',#4554,#4555,#595,.T.);
#5708=EDGE_CURVE('',#4556,#4554,#3028,.T.);
#5709=EDGE_CURVE('',#4557,#4556,#596,.T.);
#5710=EDGE_CURVE('',#4555,#4557,#3029,.T.);
#5711=EDGE_CURVE('',#4558,#4559,#597,.T.);
#5712=EDGE_CURVE('',#4560,#4558,#3030,.T.);
#5713=EDGE_CURVE('',#4561,#4560,#598,.T.);
#5714=EDGE_CURVE('',#4559,#4561,#3031,.T.);
#5715=EDGE_CURVE('',#4562,#4563,#599,.T.);
#5716=EDGE_CURVE('',#4564,#4562,#3032,.T.);
#5717=EDGE_CURVE('',#4565,#4564,#600,.T.);
#5718=EDGE_CURVE('',#4563,#4565,#3033,.T.);
#5719=EDGE_CURVE('',#4566,#4567,#601,.T.);
#5720=EDGE_CURVE('',#4568,#4566,#3034,.T.);
#5721=EDGE_CURVE('',#4569,#4568,#602,.T.);
#5722=EDGE_CURVE('',#4567,#4569,#3035,.T.);
#5723=EDGE_CURVE('',#4570,#4570,#2400,.T.);
#5724=EDGE_CURVE('',#4570,#4571,#3036,.T.);
#5725=EDGE_CURVE('',#4571,#4572,#603,.T.);
#5726=EDGE_CURVE('',#4572,#4573,#604,.T.);
#5727=EDGE_CURVE('',#4573,#4574,#3037,.T.);
#5728=EDGE_CURVE('',#4574,#4574,#2401,.T.);
#5729=EDGE_CURVE('',#4573,#4575,#605,.T.);
#5730=EDGE_CURVE('',#4575,#4571,#606,.T.);
#5731=EDGE_CURVE('',#4576,#4577,#607,.T.);
#5732=EDGE_CURVE('',#4577,#4576,#608,.T.);
#5733=EDGE_CURVE('',#4578,#4579,#2402,.T.);
#5734=EDGE_CURVE('',#4579,#4578,#2403,.T.);
#5735=EDGE_CURVE('',#4578,#4580,#3038,.T.);
#5736=EDGE_CURVE('',#4580,#4581,#609,.T.);
#5737=EDGE_CURVE('',#4581,#4582,#3039,.T.);
#5738=EDGE_CURVE('',#4582,#4582,#2404,.T.);
#5739=EDGE_CURVE('',#4581,#4583,#610,.T.);
#5740=EDGE_CURVE('',#4583,#4580,#611,.T.);
#5741=EDGE_CURVE('',#4584,#4584,#612,.T.);
#5742=EDGE_CURVE('',#4585,#4585,#2405,.T.);
#5743=EDGE_CURVE('',#4586,#4586,#2406,.T.);
#5744=EDGE_CURVE('',#4587,#4587,#2407,.T.);
#5745=EDGE_CURVE('',#4588,#4588,#2408,.T.);
#5746=EDGE_CURVE('',#4589,#4590,#2409,.T.);
#5747=EDGE_CURVE('',#4590,#4591,#3040,.T.);
#5748=EDGE_CURVE('',#4591,#4592,#613,.T.);
#5749=EDGE_CURVE('',#4592,#4593,#614,.T.);
#5750=EDGE_CURVE('',#4593,#4594,#3041,.T.);
#5751=EDGE_CURVE('',#4594,#4595,#615,.T.);
#5752=EDGE_CURVE('',#4595,#4596,#616,.T.);
#5753=EDGE_CURVE('',#4596,#4597,#3042,.T.);
#5754=EDGE_CURVE('',#4597,#4597,#2410,.T.);
#5755=EDGE_CURVE('',#4596,#4598,#617,.T.);
#5756=EDGE_CURVE('',#4598,#4594,#618,.T.);
#5757=EDGE_CURVE('',#4593,#4599,#619,.T.);
#5758=EDGE_CURVE('',#4599,#4591,#620,.T.);
#5759=EDGE_CURVE('',#4590,#4589,#2411,.T.);
#5760=EDGE_CURVE('',#4600,#4601,#621,.T.);
#5761=EDGE_CURVE('',#4601,#4600,#622,.T.);
#5762=EDGE_CURVE('',#4602,#4603,#623,.T.);
#5763=EDGE_CURVE('',#4603,#4602,#624,.T.);
#5764=EDGE_CURVE('',#4577,#4595,#3043,.T.);
#5765=EDGE_CURVE('',#4603,#4572,#3044,.T.);
#5766=EDGE_CURVE('',#4604,#4605,#625,.T.);
#5767=EDGE_CURVE('',#4605,#4592,#3045,.T.);
#5768=EDGE_CURVE('',#4605,#4604,#626,.T.);
#5769=EDGE_CURVE('',#4601,#4606,#3046,.T.);
#5770=EDGE_CURVE('',#4606,#4607,#627,.T.);
#5771=EDGE_CURVE('',#4607,#4606,#628,.T.);
#5772=EDGE_CURVE('',#4582,#4526,#2412,.T.);
#5773=EDGE_CURVE('',#4531,#4570,#2413,.T.);
#5774=EDGE_CURVE('',#4550,#4551,#2414,.T.);
#5775=EDGE_CURVE('',#4552,#4553,#2415,.T.);
#5776=EDGE_CURVE('',#4554,#4555,#2416,.T.);
#5777=EDGE_CURVE('',#4556,#4557,#2417,.T.);
#5778=EDGE_CURVE('',#4546,#4547,#2418,.T.);
#5779=EDGE_CURVE('',#4548,#4549,#2419,.T.);
#5780=EDGE_CURVE('',#4558,#4559,#2420,.T.);
#5781=EDGE_CURVE('',#4560,#4561,#2421,.T.);
#5782=EDGE_CURVE('',#4542,#4543,#2422,.T.);
#5783=EDGE_CURVE('',#4544,#4545,#2423,.T.);
#5784=EDGE_CURVE('',#4528,#4533,#2424,.T.);
#5785=EDGE_CURVE('',#4529,#4532,#2425,.T.);
#5786=EDGE_CURVE('',#4538,#4539,#2426,.T.);
#5787=EDGE_CURVE('',#4540,#4541,#2427,.T.);
#5788=EDGE_CURVE('',#4562,#4563,#2428,.T.);
#5789=EDGE_CURVE('',#4564,#4565,#2429,.T.);
#5790=EDGE_CURVE('',#4534,#4535,#2430,.T.);
#5791=EDGE_CURVE('',#4536,#4537,#2431,.T.);
#5792=EDGE_CURVE('',#4566,#4567,#2432,.T.);
#5793=EDGE_CURVE('',#4568,#4569,#2433,.T.);
#5794=EDGE_CURVE('',#4607,#4583,#629,.T.);
#5795=EDGE_CURVE('',#4604,#4584,#630,.T.);
#5796=EDGE_CURVE('',#4597,#4586,#3047,.T.);
#5797=EDGE_CURVE('',#4589,#4588,#3048,.T.);
#5798=EDGE_CURVE('',#4574,#4585,#3049,.T.);
#5799=EDGE_CURVE('',#4579,#4587,#3050,.T.);
#5800=EDGE_CURVE('',#4608,#4608,#2434,.T.);
#5801=EDGE_CURVE('',#4608,#4609,#3051,.T.);
#5802=EDGE_CURVE('',#4609,#4610,#631,.T.);
#5803=EDGE_CURVE('',#4610,#4611,#632,.T.);
#5804=EDGE_CURVE('',#4611,#4612,#3052,.T.);
#5805=EDGE_CURVE('',#4612,#4612,#2435,.T.);
#5806=EDGE_CURVE('',#4611,#4613,#633,.T.);
#5807=EDGE_CURVE('',#4613,#4609,#634,.T.);
#5808=EDGE_CURVE('',#4614,#4615,#635,.T.);
#5809=EDGE_CURVE('',#4615,#4614,#636,.T.);
#5810=EDGE_CURVE('',#4616,#4616,#2436,.T.);
#5811=EDGE_CURVE('',#4617,#4617,#2437,.T.);
#5812=EDGE_CURVE('',#4618,#4618,#2438,.T.);
#5813=EDGE_CURVE('',#4618,#4610,#3053,.T.);
#5814=EDGE_CURVE('',#4619,#4619,#2439,.T.);
#5815=EDGE_CURVE('',#4619,#4615,#3054,.T.);
#5816=EDGE_CURVE('',#4616,#4617,#3055,.T.);
#5817=EDGE_CURVE('',#4620,#4620,#2440,.T.);
#5818=EDGE_CURVE('',#4621,#4621,#2441,.T.);
#5819=EDGE_CURVE('',#4620,#4622,#3056,.T.);
#5820=EDGE_CURVE('',#4622,#4622,#2442,.T.);
#5821=EDGE_CURVE('',#4623,#4623,#2443,.T.);
#5822=EDGE_CURVE('',#4624,#4624,#2444,.T.);
#5823=EDGE_CURVE('',#4625,#4624,#2445,.T.);
#5824=EDGE_CURVE('',#4622,#4623,#2446,.T.);
#5825=EDGE_CURVE('',#4621,#4626,#3057,.T.);
#5826=EDGE_CURVE('',#4626,#4626,#2447,.T.);
#5827=EDGE_CURVE('',#4626,#4627,#3058,.T.);
#5828=EDGE_CURVE('',#4627,#4627,#2448,.T.);
#5829=EDGE_CURVE('',#4628,#4629,#3059,.T.);
#5830=EDGE_CURVE('',#4629,#4630,#3060,.T.);
#5831=EDGE_CURVE('',#4630,#4631,#3061,.T.);
#5832=EDGE_CURVE('',#4631,#4632,#3062,.T.);
#5833=EDGE_CURVE('',#4632,#4633,#3063,.T.);
#5834=EDGE_CURVE('',#4633,#4628,#3064,.T.);
#5835=EDGE_CURVE('',#4634,#4635,#3065,.T.);
#5836=EDGE_CURVE('',#4631,#4635,#3066,.T.);
#5837=EDGE_CURVE('',#4630,#4634,#3067,.T.);
#5838=EDGE_CURVE('',#4635,#4636,#3068,.T.);
#5839=EDGE_CURVE('',#4632,#4636,#3069,.T.);
#5840=EDGE_CURVE('',#4636,#4637,#3070,.T.);
#5841=EDGE_CURVE('',#4633,#4637,#3071,.T.);
#5842=EDGE_CURVE('',#4637,#4638,#3072,.T.);
#5843=EDGE_CURVE('',#4628,#4638,#3073,.T.);
#5844=EDGE_CURVE('',#4638,#4639,#3074,.T.);
#5845=EDGE_CURVE('',#4629,#4639,#3075,.T.);
#5846=EDGE_CURVE('',#4639,#4634,#3076,.T.);
#5847=EDGE_CURVE('',#4640,#4641,#2449,.T.);
#5848=EDGE_CURVE('',#4641,#4640,#3077,.T.);
#5849=EDGE_CURVE('',#4642,#4643,#3078,.T.);
#5850=EDGE_CURVE('',#4642,#4643,#2450,.T.);
#5851=EDGE_CURVE('',#4640,#4642,#202,.T.);
#5852=EDGE_CURVE('',#4642,#4643,#637,.T.);
#5853=EDGE_CURVE('',#4640,#4641,#638,.T.);
#5854=EDGE_CURVE('',#4644,#4645,#2451,.T.);
#5855=EDGE_CURVE('',#4645,#4644,#2452,.T.);
#5856=EDGE_CURVE('',#4644,#4646,#3079,.T.);
#5857=EDGE_CURVE('',#4646,#4646,#2453,.T.);
#5858=EDGE_CURVE('',#4647,#4647,#2454,.T.);
#5859=EDGE_CURVE('',#4648,#4648,#2455,.T.);
#5860=EDGE_CURVE('',#4649,#4649,#2456,.T.);
#5861=EDGE_CURVE('',#4647,#4650,#3080,.T.);
#5862=EDGE_CURVE('',#4650,#4650,#2457,.T.);
#5863=EDGE_CURVE('',#4651,#4652,#3081,.T.);
#5864=EDGE_CURVE('',#4653,#4651,#3082,.T.);
#5865=EDGE_CURVE('',#4654,#4653,#3083,.T.);
#5866=EDGE_CURVE('',#4652,#4654,#3084,.T.);
#5867=EDGE_CURVE('',#4655,#4652,#3085,.T.);
#5868=EDGE_CURVE('',#4656,#4655,#3086,.T.);
#5869=EDGE_CURVE('',#4656,#4651,#3087,.T.);
#5870=EDGE_CURVE('',#4657,#4656,#3088,.T.);
#5871=EDGE_CURVE('',#4657,#4653,#3089,.T.);
#5872=EDGE_CURVE('',#4658,#4657,#3090,.T.);
#5873=EDGE_CURVE('',#4658,#4654,#3091,.T.);
#5874=EDGE_CURVE('',#4655,#4658,#3092,.T.);
#5875=EDGE_CURVE('',#4645,#4648,#2458,.T.);
#5876=EDGE_CURVE('',#4659,#4660,#3093,.T.);
#5877=EDGE_CURVE('',#4660,#4661,#3094,.T.);
#5878=EDGE_CURVE('',#4661,#4662,#3095,.T.);
#5879=EDGE_CURVE('',#4662,#4659,#3096,.T.);
#5880=EDGE_CURVE('',#4663,#4664,#3097,.T.);
#5881=EDGE_CURVE('',#4664,#4665,#3098,.T.);
#5882=EDGE_CURVE('',#4665,#4666,#3099,.T.);
#5883=EDGE_CURVE('',#4666,#4667,#3100,.T.);
#5884=EDGE_CURVE('',#4667,#4668,#3101,.T.);
#5885=EDGE_CURVE('',#4668,#4669,#3102,.T.);
#5886=EDGE_CURVE('',#4669,#4670,#3103,.T.);
#5887=EDGE_CURVE('',#4670,#4671,#3104,.T.);
#5888=EDGE_CURVE('',#4671,#4672,#3105,.T.);
#5889=EDGE_CURVE('',#4672,#4673,#3106,.T.);
#5890=EDGE_CURVE('',#4673,#4674,#3107,.T.);
#5891=EDGE_CURVE('',#4674,#4663,#3108,.T.);
#5892=EDGE_CURVE('',#4675,#4676,#3109,.T.);
#5893=EDGE_CURVE('',#4660,#4676,#3110,.T.);
#5894=EDGE_CURVE('',#4659,#4675,#3111,.T.);
#5895=EDGE_CURVE('',#4676,#4677,#3112,.T.);
#5896=EDGE_CURVE('',#4661,#4677,#3113,.T.);
#5897=EDGE_CURVE('',#4677,#4678,#3114,.T.);
#5898=EDGE_CURVE('',#4662,#4678,#3115,.T.);
#5899=EDGE_CURVE('',#4678,#4675,#3116,.T.);
#5900=EDGE_CURVE('',#4679,#4680,#3117,.T.);
#5901=EDGE_CURVE('',#4681,#4679,#3118,.T.);
#5902=EDGE_CURVE('',#4682,#4681,#3119,.T.);
#5903=EDGE_CURVE('',#4683,#4682,#3120,.T.);
#5904=EDGE_CURVE('',#4684,#4683,#3121,.T.);
#5905=EDGE_CURVE('',#4685,#4684,#3122,.T.);
#5906=EDGE_CURVE('',#4686,#4685,#3123,.T.);
#5907=EDGE_CURVE('',#4687,#4686,#3124,.T.);
#5908=EDGE_CURVE('',#4688,#4687,#3125,.T.);
#5909=EDGE_CURVE('',#4689,#4688,#3126,.T.);
#5910=EDGE_CURVE('',#4690,#4689,#3127,.T.);
#5911=EDGE_CURVE('',#4680,#4690,#3128,.T.);
#5912=EDGE_CURVE('',#4691,#4663,#3129,.T.);
#5913=EDGE_CURVE('',#4691,#4692,#3130,.T.);
#5914=EDGE_CURVE('',#4692,#4664,#3131,.T.);
#5915=EDGE_CURVE('',#4692,#4693,#3132,.T.);
#5916=EDGE_CURVE('',#4693,#4665,#3133,.T.);
#5917=EDGE_CURVE('',#4693,#4694,#3134,.T.);
#5918=EDGE_CURVE('',#4694,#4666,#3135,.T.);
#5919=EDGE_CURVE('',#4694,#4695,#3136,.T.);
#5920=EDGE_CURVE('',#4695,#4667,#3137,.T.);
#5921=EDGE_CURVE('',#4695,#4696,#3138,.T.);
#5922=EDGE_CURVE('',#4696,#4668,#3139,.T.);
#5923=EDGE_CURVE('',#4696,#4697,#3140,.T.);
#5924=EDGE_CURVE('',#4697,#4669,#3141,.T.);
#5925=EDGE_CURVE('',#4697,#4698,#3142,.T.);
#5926=EDGE_CURVE('',#4698,#4670,#3143,.T.);
#5927=EDGE_CURVE('',#4698,#4699,#3144,.T.);
#5928=EDGE_CURVE('',#4699,#4671,#3145,.T.);
#5929=EDGE_CURVE('',#4699,#4700,#3146,.T.);
#5930=EDGE_CURVE('',#4700,#4672,#3147,.T.);
#5931=EDGE_CURVE('',#4700,#4701,#3148,.T.);
#5932=EDGE_CURVE('',#4701,#4673,#3149,.T.);
#5933=EDGE_CURVE('',#4701,#4702,#3150,.T.);
#5934=EDGE_CURVE('',#4702,#4674,#3151,.T.);
#5935=EDGE_CURVE('',#4702,#4691,#3152,.T.);
#5936=EDGE_CURVE('',#4703,#4680,#3153,.T.);
#5937=EDGE_CURVE('',#4704,#4703,#3154,.T.);
#5938=EDGE_CURVE('',#4704,#4679,#3155,.T.);
#5939=EDGE_CURVE('',#4705,#4704,#3156,.T.);
#5940=EDGE_CURVE('',#4705,#4681,#3157,.T.);
#5941=EDGE_CURVE('',#4706,#4705,#3158,.T.);
#5942=EDGE_CURVE('',#4706,#4682,#3159,.T.);
#5943=EDGE_CURVE('',#4707,#4706,#3160,.T.);
#5944=EDGE_CURVE('',#4707,#4683,#3161,.T.);
#5945=EDGE_CURVE('',#4708,#4707,#3162,.T.);
#5946=EDGE_CURVE('',#4708,#4684,#3163,.T.);
#5947=EDGE_CURVE('',#4709,#4708,#3164,.T.);
#5948=EDGE_CURVE('',#4709,#4685,#3165,.T.);
#5949=EDGE_CURVE('',#4710,#4709,#3166,.T.);
#5950=EDGE_CURVE('',#4710,#4686,#3167,.T.);
#5951=EDGE_CURVE('',#4711,#4710,#3168,.T.);
#5952=EDGE_CURVE('',#4711,#4687,#3169,.T.);
#5953=EDGE_CURVE('',#4712,#4711,#3170,.T.);
#5954=EDGE_CURVE('',#4712,#4688,#3171,.T.);
#5955=EDGE_CURVE('',#4713,#4712,#3172,.T.);
#5956=EDGE_CURVE('',#4713,#4689,#3173,.T.);
#5957=EDGE_CURVE('',#4714,#4713,#3174,.T.);
#5958=EDGE_CURVE('',#4714,#4690,#3175,.T.);
#5959=EDGE_CURVE('',#4703,#4714,#3176,.T.);
#5960=EDGE_CURVE('',#4715,#4715,#2459,.T.);
#5961=EDGE_CURVE('',#4715,#4716,#2460,.T.);
#5962=EDGE_CURVE('',#4716,#4716,#2461,.T.);
#5963=EDGE_CURVE('',#4717,#4717,#2462,.T.);
#5964=EDGE_CURVE('',#4717,#4718,#3177,.T.);
#5965=EDGE_CURVE('',#4718,#4718,#2463,.T.);
#5966=EDGE_CURVE('',#4719,#4719,#2464,.T.);
#5967=EDGE_CURVE('',#4720,#4720,#2465,.T.);
#5968=EDGE_CURVE('',#4721,#4721,#2466,.T.);
#5969=EDGE_CURVE('',#4722,#4722,#2467,.T.);
#5970=EDGE_CURVE('',#4721,#4719,#3178,.T.);
#5971=EDGE_CURVE('',#4720,#4722,#3179,.T.);
#5972=EDGE_CURVE('',#4723,#4723,#2468,.T.);
#5973=EDGE_CURVE('',#4723,#4724,#3180,.T.);
#5974=EDGE_CURVE('',#4724,#4724,#2469,.T.);
#5975=EDGE_CURVE('',#4725,#4725,#2470,.T.);
#5976=EDGE_CURVE('',#4725,#4726,#3181,.T.);
#5977=EDGE_CURVE('',#4726,#4726,#2471,.T.);
#5978=EDGE_CURVE('',#4727,#4727,#2472,.T.);
#5979=EDGE_CURVE('',#4728,#4728,#2473,.T.);
#5980=EDGE_CURVE('',#4728,#4729,#3182,.T.);
#5981=EDGE_CURVE('',#4729,#4729,#2474,.T.);
#5982=EDGE_CURVE('',#4730,#4730,#2475,.T.);
#5983=EDGE_CURVE('',#4730,#4727,#3183,.T.);
#5984=EDGE_CURVE('',#4731,#4732,#2476,.T.);
#5985=EDGE_CURVE('',#4732,#4733,#639,.T.);
#5986=EDGE_CURVE('',#4733,#4734,#3184,.T.);
#5987=EDGE_CURVE('',#4734,#4735,#640,.T.);
#5988=EDGE_CURVE('',#4735,#4736,#2477,.T.);
#5989=EDGE_CURVE('',#4736,#4737,#641,.T.);
#5990=EDGE_CURVE('',#4737,#4738,#3185,.T.);
#5991=EDGE_CURVE('',#4738,#4731,#642,.T.);
#5992=EDGE_CURVE('',#4739,#4740,#3186,.T.);
#5993=EDGE_CURVE('',#4740,#4741,#643,.T.);
#5994=EDGE_CURVE('',#4741,#4742,#2478,.T.);
#5995=EDGE_CURVE('',#4742,#4743,#644,.T.);
#5996=EDGE_CURVE('',#4743,#4744,#3187,.T.);
#5997=EDGE_CURVE('',#4744,#4745,#645,.T.);
#5998=EDGE_CURVE('',#4745,#4746,#2479,.T.);
#5999=EDGE_CURVE('',#4746,#4739,#646,.T.);
#6000=EDGE_CURVE('',#4747,#4748,#3188,.T.);
#6001=EDGE_CURVE('',#4748,#4749,#647,.T.);
#6002=EDGE_CURVE('',#4749,#4750,#2480,.T.);
#6003=EDGE_CURVE('',#4750,#4751,#648,.T.);
#6004=EDGE_CURVE('',#4751,#4752,#3189,.T.);
#6005=EDGE_CURVE('',#4752,#4753,#649,.T.);
#6006=EDGE_CURVE('',#4753,#4754,#2481,.T.);
#6007=EDGE_CURVE('',#4754,#4747,#650,.T.);
#6008=EDGE_CURVE('',#4755,#4756,#3190,.T.);
#6009=EDGE_CURVE('',#4756,#4757,#651,.T.);
#6010=EDGE_CURVE('',#4757,#4758,#2482,.T.);
#6011=EDGE_CURVE('',#4758,#4759,#652,.T.);
#6012=EDGE_CURVE('',#4759,#4760,#3191,.T.);
#6013=EDGE_CURVE('',#4760,#4761,#653,.T.);
#6014=EDGE_CURVE('',#4761,#4762,#2483,.T.);
#6015=EDGE_CURVE('',#4762,#4763,#2484,.T.);
#6016=EDGE_CURVE('',#4763,#4755,#654,.T.);
#6017=EDGE_CURVE('',#4764,#4765,#2485,.T.);
#6018=EDGE_CURVE('',#4765,#4766,#655,.T.);
#6019=EDGE_CURVE('',#4766,#4767,#3192,.T.);
#6020=EDGE_CURVE('',#4767,#4768,#656,.T.);
#6021=EDGE_CURVE('',#4768,#4769,#2486,.T.);
#6022=EDGE_CURVE('',#4769,#4770,#657,.T.);
#6023=EDGE_CURVE('',#4770,#4771,#3193,.T.);
#6024=EDGE_CURVE('',#4771,#4764,#658,.T.);
#6025=EDGE_CURVE('',#4772,#4773,#3194,.T.);
#6026=EDGE_CURVE('',#4773,#4774,#659,.T.);
#6027=EDGE_CURVE('',#4774,#4775,#2487,.T.);
#6028=EDGE_CURVE('',#4775,#4776,#660,.T.);
#6029=EDGE_CURVE('',#4776,#4777,#3195,.T.);
#6030=EDGE_CURVE('',#4777,#4778,#661,.T.);
#6031=EDGE_CURVE('',#4778,#4779,#2488,.T.);
#6032=EDGE_CURVE('',#4779,#4772,#662,.T.);
#6033=EDGE_CURVE('',#4780,#4781,#3196,.T.);
#6034=EDGE_CURVE('',#4781,#4782,#663,.T.);
#6035=EDGE_CURVE('',#4782,#4783,#2489,.T.);
#6036=EDGE_CURVE('',#4783,#4784,#664,.T.);
#6037=EDGE_CURVE('',#4784,#4785,#3197,.T.);
#6038=EDGE_CURVE('',#4785,#4786,#665,.T.);
#6039=EDGE_CURVE('',#4786,#4787,#2490,.T.);
#6040=EDGE_CURVE('',#4787,#4780,#666,.T.);
#6041=EDGE_CURVE('',#4788,#4789,#3198,.T.);
#6042=EDGE_CURVE('',#4789,#4790,#667,.T.);
#6043=EDGE_CURVE('',#4790,#4791,#2491,.T.);
#6044=EDGE_CURVE('',#4791,#4792,#668,.T.);
#6045=EDGE_CURVE('',#4792,#4793,#3199,.T.);
#6046=EDGE_CURVE('',#4793,#4794,#669,.T.);
#6047=EDGE_CURVE('',#4794,#4795,#2492,.T.);
#6048=EDGE_CURVE('',#4795,#4788,#670,.T.);
#6049=EDGE_CURVE('',#4796,#4797,#3200,.T.);
#6050=EDGE_CURVE('',#4797,#4798,#671,.T.);
#6051=EDGE_CURVE('',#4798,#4799,#2493,.T.);
#6052=EDGE_CURVE('',#4799,#4800,#672,.T.);
#6053=EDGE_CURVE('',#4800,#4801,#3201,.T.);
#6054=EDGE_CURVE('',#4801,#4802,#673,.T.);
#6055=EDGE_CURVE('',#4802,#4803,#2494,.T.);
#6056=EDGE_CURVE('',#4803,#4796,#674,.T.);
#6057=EDGE_CURVE('',#4741,#4750,#2495,.T.);
#6058=EDGE_CURVE('',#4749,#4758,#2496,.T.);
#6059=EDGE_CURVE('',#4757,#4765,#2497,.T.);
#6060=EDGE_CURVE('',#4764,#4775,#2498,.T.);
#6061=EDGE_CURVE('',#4774,#4783,#2499,.T.);
#6062=EDGE_CURVE('',#4782,#4791,#2500,.T.);
#6063=EDGE_CURVE('',#4790,#4799,#2501,.T.);
#6064=EDGE_CURVE('',#4798,#4804,#2502,.T.);
#6065=EDGE_CURVE('',#4805,#4804,#2503,.T.);
#6066=EDGE_CURVE('',#4805,#4732,#2504,.T.);
#6067=EDGE_CURVE('',#4731,#4742,#2505,.T.);
#6068=EDGE_CURVE('',#4806,#4806,#2506,.T.);
#6069=EDGE_CURVE('',#4807,#4807,#2507,.T.);
#6070=EDGE_CURVE('',#4807,#4808,#3202,.T.);
#6071=EDGE_CURVE('',#4808,#4808,#2508,.T.);
#6072=EDGE_CURVE('',#4809,#4809,#2509,.T.);
#6073=EDGE_CURVE('',#4809,#4810,#3203,.T.);
#6074=EDGE_CURVE('',#4810,#4810,#2510,.T.);
#6075=EDGE_CURVE('',#4811,#4812,#3204,.T.);
#6076=EDGE_CURVE('',#4812,#4805,#675,.T.);
#6077=EDGE_CURVE('',#4804,#4813,#676,.T.);
#6078=EDGE_CURVE('',#4813,#4814,#3205,.T.);
#6079=EDGE_CURVE('',#4814,#4815,#677,.T.);
#6080=EDGE_CURVE('',#4815,#4816,#2511,.T.);
#6081=EDGE_CURVE('',#4816,#4811,#678,.T.);
#6082=EDGE_CURVE('',#4817,#4817,#2512,.T.);
#6083=EDGE_CURVE('',#4818,#4818,#2513,.T.);
#6084=EDGE_CURVE('',#4819,#4820,#2514,.T.);
#6085=EDGE_CURVE('',#4820,#4819,#2515,.T.);
#6086=EDGE_CURVE('',#4819,#4817,#3206,.T.);
#6087=EDGE_CURVE('',#4820,#4821,#3207,.T.);
#6088=EDGE_CURVE('',#4821,#4821,#2516,.T.);
#6089=EDGE_CURVE('',#4822,#4823,#679,.T.);
#6090=EDGE_CURVE('',#4823,#4822,#680,.T.);
#6091=EDGE_CURVE('',#4824,#4825,#681,.T.);
#6092=EDGE_CURVE('',#4825,#4824,#682,.T.);
#6093=EDGE_CURVE('',#4826,#4827,#683,.T.);
#6094=EDGE_CURVE('',#4827,#4826,#684,.T.);
#6095=EDGE_CURVE('',#4828,#4829,#685,.T.);
#6096=EDGE_CURVE('',#4829,#4828,#686,.T.);
#6097=EDGE_CURVE('',#4830,#4831,#687,.T.);
#6098=EDGE_CURVE('',#4831,#4830,#688,.T.);
#6099=EDGE_CURVE('',#4832,#4832,#2517,.T.);
#6100=EDGE_CURVE('',#4832,#4833,#3208,.T.);
#6101=EDGE_CURVE('',#4833,#4834,#2518,.T.);
#6102=EDGE_CURVE('',#4834,#4833,#2519,.T.);
#6103=EDGE_CURVE('',#4735,#4816,#689,.T.);
#6104=EDGE_CURVE('',#4815,#4803,#690,.T.);
#6105=EDGE_CURVE('',#4802,#4795,#691,.T.);
#6106=EDGE_CURVE('',#4794,#4787,#692,.T.);
#6107=EDGE_CURVE('',#4786,#4779,#693,.T.);
#6108=EDGE_CURVE('',#4778,#4769,#694,.T.);
#6109=EDGE_CURVE('',#4768,#4763,#695,.T.);
#6110=EDGE_CURVE('',#4762,#4834,#3209,.T.);
#6111=EDGE_CURVE('',#4761,#4754,#696,.T.);
#6112=EDGE_CURVE('',#4753,#4746,#697,.T.);
#6113=EDGE_CURVE('',#4745,#4736,#698,.T.);
#6114=EDGE_CURVE('',#4835,#4835,#2520,.T.);
#6115=EDGE_CURVE('',#4835,#4818,#3210,.T.);
#6116=EDGE_CURVE('',#4836,#4837,#699,.T.);
#6117=EDGE_CURVE('',#4837,#4836,#700,.T.);
#6118=EDGE_CURVE('',#4838,#4839,#701,.T.);
#6119=EDGE_CURVE('',#4839,#4838,#702,.T.);
#6120=EDGE_CURVE('',#4840,#4841,#703,.T.);
#6121=EDGE_CURVE('',#4841,#4840,#704,.T.);
#6122=EDGE_CURVE('',#4842,#4843,#705,.T.);
#6123=EDGE_CURVE('',#4843,#4842,#706,.T.);
#6124=EDGE_CURVE('',#4844,#4845,#707,.T.);
#6125=EDGE_CURVE('',#4845,#4844,#708,.T.);
#6126=EDGE_CURVE('',#4831,#4845,#3211,.T.);
#6127=EDGE_CURVE('',#4829,#4843,#3212,.T.);
#6128=EDGE_CURVE('',#4827,#4841,#3213,.T.);
#6129=EDGE_CURVE('',#4825,#4839,#3214,.T.);
#6130=EDGE_CURVE('',#4823,#4837,#3215,.T.);
#6131=EDGE_CURVE('',#4846,#4846,#2521,.T.);
#6132=EDGE_CURVE('',#4846,#4806,#3216,.T.);
#6133=EDGE_CURVE('',#4808,#4846,#3217,.T.);
#6134=EDGE_CURVE('',#4847,#4847,#2522,.T.);
#6135=EDGE_CURVE('',#4847,#4848,#3218,.T.);
#6136=EDGE_CURVE('',#4848,#4848,#2523,.T.);
#6137=EDGE_CURVE('',#4849,#4850,#3219,.T.);
#6138=EDGE_CURVE('',#4850,#4851,#2524,.T.);
#6139=EDGE_CURVE('',#4851,#4852,#3220,.T.);
#6140=EDGE_CURVE('',#4852,#4849,#709,.T.);
#6141=EDGE_CURVE('',#4853,#4854,#3221,.T.);
#6142=EDGE_CURVE('',#4854,#4855,#2525,.T.);
#6143=EDGE_CURVE('',#4855,#4856,#3222,.T.);
#6144=EDGE_CURVE('',#4856,#4853,#710,.T.);
#6145=EDGE_CURVE('',#4857,#4858,#3223,.T.);
#6146=EDGE_CURVE('',#4858,#4859,#2526,.T.);
#6147=EDGE_CURVE('',#4859,#4860,#3224,.T.);
#6148=EDGE_CURVE('',#4860,#4857,#711,.T.);
#6149=EDGE_CURVE('',#4861,#4862,#3225,.T.);
#6150=EDGE_CURVE('',#4862,#4863,#2527,.T.);
#6151=EDGE_CURVE('',#4863,#4864,#3226,.T.);
#6152=EDGE_CURVE('',#4864,#4861,#712,.T.);
#6153=EDGE_CURVE('',#4865,#4866,#3227,.T.);
#6154=EDGE_CURVE('',#4866,#4867,#2528,.T.);
#6155=EDGE_CURVE('',#4867,#4868,#3228,.T.);
#6156=EDGE_CURVE('',#4868,#4865,#713,.T.);
#6157=EDGE_CURVE('',#4869,#4870,#714,.T.);
#6158=EDGE_CURVE('',#4870,#4871,#3229,.T.);
#6159=EDGE_CURVE('',#4871,#4872,#2529,.T.);
#6160=EDGE_CURVE('',#4872,#4869,#3230,.T.);
#6161=EDGE_CURVE('',#4873,#4874,#3231,.T.);
#6162=EDGE_CURVE('',#4874,#4875,#2530,.T.);
#6163=EDGE_CURVE('',#4875,#4876,#3232,.T.);
#6164=EDGE_CURVE('',#4876,#4873,#715,.T.);
#6165=EDGE_CURVE('',#4877,#4878,#3233,.T.);
#6166=EDGE_CURVE('',#4878,#4879,#2531,.T.);
#6167=EDGE_CURVE('',#4879,#4880,#3234,.T.);
#6168=EDGE_CURVE('',#4880,#4877,#716,.T.);
#6169=EDGE_CURVE('',#4881,#4882,#3235,.T.);
#6170=EDGE_CURVE('',#4882,#4883,#2532,.T.);
#6171=EDGE_CURVE('',#4883,#4884,#3236,.T.);
#6172=EDGE_CURVE('',#4884,#4881,#717,.T.);
#6173=EDGE_CURVE('',#4885,#4886,#3237,.T.);
#6174=EDGE_CURVE('',#4886,#4887,#2533,.T.);
#6175=EDGE_CURVE('',#4887,#4888,#3238,.T.);
#6176=EDGE_CURVE('',#4888,#4885,#718,.T.);
#6177=EDGE_CURVE('',#4881,#4752,#719,.T.);
#6178=EDGE_CURVE('',#4739,#4884,#410,.T.);
#6179=EDGE_CURVE('',#4882,#4751,#720,.T.);
#6180=EDGE_CURVE('',#4740,#4883,#721,.T.);
#6181=EDGE_CURVE('',#4877,#4760,#722,.T.);
#6182=EDGE_CURVE('',#4747,#4880,#411,.T.);
#6183=EDGE_CURVE('',#4878,#4759,#723,.T.);
#6184=EDGE_CURVE('',#4748,#4879,#724,.T.);
#6185=EDGE_CURVE('',#4873,#4767,#725,.T.);
#6186=EDGE_CURVE('',#4755,#4876,#726,.T.);
#6187=EDGE_CURVE('',#4874,#4766,#727,.T.);
#6188=EDGE_CURVE('',#4756,#4875,#728,.T.);
#6189=EDGE_CURVE('',#4870,#4777,#729,.T.);
#6190=EDGE_CURVE('',#4770,#4869,#412,.T.);
#6191=EDGE_CURVE('',#4871,#4776,#730,.T.);
#6192=EDGE_CURVE('',#4771,#4872,#731,.T.);
#6193=EDGE_CURVE('',#4865,#4785,#732,.T.);
#6194=EDGE_CURVE('',#4772,#4868,#733,.T.);
#6195=EDGE_CURVE('',#4866,#4784,#734,.T.);
#6196=EDGE_CURVE('',#4773,#4867,#735,.T.);
#6197=EDGE_CURVE('',#4861,#4793,#736,.T.);
#6198=EDGE_CURVE('',#4780,#4864,#413,.T.);
#6199=EDGE_CURVE('',#4862,#4792,#737,.T.);
#6200=EDGE_CURVE('',#4781,#4863,#738,.T.);
#6201=EDGE_CURVE('',#4857,#4801,#739,.T.);
#6202=EDGE_CURVE('',#4788,#4860,#414,.T.);
#6203=EDGE_CURVE('',#4858,#4800,#740,.T.);
#6204=EDGE_CURVE('',#4789,#4859,#741,.T.);
#6205=EDGE_CURVE('',#4853,#4814,#742,.T.);
#6206=EDGE_CURVE('',#4796,#4856,#743,.T.);
#6207=EDGE_CURVE('',#4854,#4813,#744,.T.);
#6208=EDGE_CURVE('',#4797,#4855,#745,.T.);
#6209=EDGE_CURVE('',#4849,#4734,#746,.T.);
#6210=EDGE_CURVE('',#4811,#4852,#415,.T.);
#6211=EDGE_CURVE('',#4850,#4733,#747,.T.);
#6212=EDGE_CURVE('',#4812,#4851,#748,.T.);
#6213=EDGE_CURVE('',#4885,#4744,#749,.T.);
#6214=EDGE_CURVE('',#4737,#4888,#750,.T.);
#6215=EDGE_CURVE('',#4886,#4743,#751,.T.);
#6216=EDGE_CURVE('',#4738,#4887,#752,.T.);
#6217=EDGE_CURVE('',#4889,#4889,#2534,.T.);
#6218=EDGE_CURVE('',#4890,#4890,#2535,.T.);
#6219=EDGE_CURVE('',#4891,#4891,#2536,.T.);
#6220=EDGE_CURVE('',#4892,#4893,#3239,.T.);
#6221=EDGE_CURVE('',#4894,#4892,#3240,.T.);
#6222=EDGE_CURVE('',#4895,#4894,#3241,.T.);
#6223=EDGE_CURVE('',#4896,#4895,#3242,.T.);
#6224=EDGE_CURVE('',#4897,#4896,#3243,.T.);
#6225=EDGE_CURVE('',#4898,#4897,#3244,.T.);
#6226=EDGE_CURVE('',#4899,#4898,#3245,.T.);
#6227=EDGE_CURVE('',#4900,#4899,#3246,.T.);
#6228=EDGE_CURVE('',#4901,#4900,#3247,.T.);
#6229=EDGE_CURVE('',#4902,#4901,#3248,.T.);
#6230=EDGE_CURVE('',#4903,#4902,#3249,.T.);
#6231=EDGE_CURVE('',#4904,#4903,#3250,.T.);
#6232=EDGE_CURVE('',#4905,#4904,#3251,.T.);
#6233=EDGE_CURVE('',#4906,#4905,#3252,.T.);
#6234=EDGE_CURVE('',#4907,#4906,#3253,.T.);
#6235=EDGE_CURVE('',#4908,#4907,#3254,.T.);
#6236=EDGE_CURVE('',#4909,#4908,#3255,.T.);
#6237=EDGE_CURVE('',#4910,#4909,#3256,.T.);
#6238=EDGE_CURVE('',#4911,#4910,#3257,.T.);
#6239=EDGE_CURVE('',#4912,#4911,#3258,.T.);
#6240=EDGE_CURVE('',#4913,#4912,#3259,.T.);
#6241=EDGE_CURVE('',#4914,#4913,#3260,.T.);
#6242=EDGE_CURVE('',#4915,#4914,#3261,.T.);
#6243=EDGE_CURVE('',#4893,#4915,#3262,.T.);
#6244=EDGE_CURVE('',#4916,#4917,#3263,.T.);
#6245=EDGE_CURVE('',#4916,#4903,#3264,.T.);
#6246=EDGE_CURVE('',#4917,#4902,#3265,.T.);
#6247=EDGE_CURVE('',#4918,#4919,#3266,.T.);
#6248=EDGE_CURVE('',#4918,#4907,#3267,.T.);
#6249=EDGE_CURVE('',#4919,#4906,#3268,.T.);
#6250=EDGE_CURVE('',#4920,#4921,#3269,.T.);
#6251=EDGE_CURVE('',#4920,#4911,#3270,.T.);
#6252=EDGE_CURVE('',#4921,#4910,#3271,.T.);
#6253=EDGE_CURVE('',#4892,#4922,#3272,.T.);
#6254=EDGE_CURVE('',#4923,#4922,#3273,.T.);
#6255=EDGE_CURVE('',#4923,#4894,#3274,.T.);
#6256=EDGE_CURVE('',#4924,#4923,#3275,.T.);
#6257=EDGE_CURVE('',#4924,#4895,#3276,.T.);
#6258=EDGE_CURVE('',#4925,#4926,#3277,.T.);
#6259=EDGE_CURVE('',#4925,#4899,#3278,.T.);
#6260=EDGE_CURVE('',#4926,#4898,#3279,.T.);
#6261=EDGE_CURVE('',#4927,#4928,#2537,.T.);
#6262=EDGE_CURVE('',#4928,#4927,#2538,.T.);
#6263=EDGE_CURVE('',#4927,#4890,#3280,.T.);
#6264=EDGE_CURVE('',#4929,#4930,#2539,.T.);
#6265=EDGE_CURVE('',#4930,#4929,#2540,.T.);
#6266=EDGE_CURVE('',#4929,#4931,#3281,.T.);
#6267=EDGE_CURVE('',#4931,#4931,#2541,.T.);
#6268=EDGE_CURVE('',#4932,#4933,#3282,.T.);
#6269=EDGE_CURVE('',#4933,#4934,#3283,.T.);
#6270=EDGE_CURVE('',#4934,#4920,#3284,.T.);
#6271=EDGE_CURVE('',#4921,#4935,#3285,.T.);
#6272=EDGE_CURVE('',#4935,#4936,#3286,.T.);
#6273=EDGE_CURVE('',#4936,#4918,#3287,.T.);
#6274=EDGE_CURVE('',#4919,#4937,#3288,.T.);
#6275=EDGE_CURVE('',#4937,#4938,#3289,.T.);
#6276=EDGE_CURVE('',#4938,#4916,#3290,.T.);
#6277=EDGE_CURVE('',#4917,#4939,#3291,.T.);
#6278=EDGE_CURVE('',#4939,#4940,#3292,.T.);
#6279=EDGE_CURVE('',#4940,#4925,#3293,.T.);
#6280=EDGE_CURVE('',#4926,#4941,#3294,.T.);
#6281=EDGE_CURVE('',#4941,#4942,#3295,.T.);
#6282=EDGE_CURVE('',#4942,#4924,#3296,.T.);
#6283=EDGE_CURVE('',#4922,#4943,#3297,.T.);
#6284=EDGE_CURVE('',#4943,#4944,#3298,.T.);
#6285=EDGE_CURVE('',#4944,#4932,#3299,.T.);
#6286=EDGE_CURVE('',#4945,#4945,#2542,.T.);
#6287=EDGE_CURVE('',#4905,#4937,#3300,.T.);
#6288=EDGE_CURVE('',#4909,#4935,#3301,.T.);
#6289=EDGE_CURVE('',#4913,#4933,#3302,.T.);
#6290=EDGE_CURVE('',#4932,#4914,#3303,.T.);
#6291=EDGE_CURVE('',#4944,#4915,#3304,.T.);
#6292=EDGE_CURVE('',#4897,#4941,#3305,.T.);
#6293=EDGE_CURVE('',#4901,#4939,#3306,.T.);
#6294=EDGE_CURVE('',#4940,#4900,#3307,.T.);
#6295=EDGE_CURVE('',#4942,#4896,#3308,.T.);
#6296=EDGE_CURVE('',#4943,#4893,#3309,.T.);
#6297=EDGE_CURVE('',#4934,#4912,#3310,.T.);
#6298=EDGE_CURVE('',#4936,#4908,#3311,.T.);
#6299=EDGE_CURVE('',#4938,#4904,#3312,.T.);
#6300=EDGE_CURVE('',#4928,#4945,#3313,.T.);
#6301=EDGE_CURVE('',#4930,#4891,#2543,.T.);
#6302=EDGE_CURVE('',#4931,#4889,#3314,.T.);
#6303=EDGE_CURVE('',#4946,#4947,#2544,.T.);
#6304=EDGE_CURVE('',#4948,#4947,#203,.T.);
#6305=EDGE_CURVE('',#4949,#4948,#204,.T.);
#6306=EDGE_CURVE('',#4950,#4949,#2545,.T.);
#6307=EDGE_CURVE('',#4950,#4946,#205,.T.);
#6308=EDGE_CURVE('',#4951,#4950,#2546,.T.);
#6309=EDGE_CURVE('',#4951,#4949,#206,.T.);
#6310=EDGE_CURVE('',#4949,#4948,#207,.T.);
#6311=EDGE_CURVE('',#4948,#4946,#2547,.T.);
#6312=EDGE_CURVE('',#4952,#4951,#2548,.T.);
#6313=EDGE_CURVE('',#4952,#4953,#208,.T.);
#6314=EDGE_CURVE('',#4953,#4948,#2549,.T.);
#6315=EDGE_CURVE('',#4949,#4952,#2550,.T.);
#6316=EDGE_CURVE('',#4947,#4953,#2551,.T.);
#6317=EDGE_CURVE('',#4954,#4954,#2552,.T.);
#6318=EDGE_CURVE('',#4955,#4955,#2553,.T.);
#6319=EDGE_CURVE('',#4954,#4956,#3315,.T.);
#6320=EDGE_CURVE('',#4956,#4956,#2554,.T.);
#6321=EDGE_CURVE('',#4956,#4957,#2555,.T.);
#6322=EDGE_CURVE('',#4957,#4957,#2556,.T.);
#6323=EDGE_CURVE('',#4957,#4958,#3316,.T.);
#6324=EDGE_CURVE('',#4958,#4958,#2557,.T.);
#6325=EDGE_CURVE('',#4959,#4959,#2558,.T.);
#6326=EDGE_CURVE('',#4959,#4960,#3317,.T.);
#6327=EDGE_CURVE('',#4960,#4960,#2559,.T.);
#6328=EDGE_CURVE('',#4961,#4961,#2560,.T.);
#6329=EDGE_CURVE('',#4961,#4962,#3318,.T.);
#6330=EDGE_CURVE('',#4962,#4963,#2561,.T.);
#6331=EDGE_CURVE('',#4963,#4962,#2562,.T.);
#6332=EDGE_CURVE('',#4964,#4965,#2563,.T.);
#6333=EDGE_CURVE('',#4965,#4964,#2564,.T.);
#6334=EDGE_CURVE('',#4964,#4963,#3319,.T.);
#6335=EDGE_CURVE('',#4965,#4966,#3320,.T.);
#6336=EDGE_CURVE('',#4966,#4967,#2565,.T.);
#6337=EDGE_CURVE('',#4967,#4966,#2566,.T.);
#6338=EDGE_CURVE('',#4968,#4969,#2567,.T.);
#6339=EDGE_CURVE('',#4969,#4968,#2568,.T.);
#6340=EDGE_CURVE('',#4968,#4967,#3321,.T.);
#6341=EDGE_CURVE('',#4969,#4970,#3322,.T.);
#6342=EDGE_CURVE('',#4970,#4970,#2569,.T.);
#6343=EDGE_CURVE('',#4971,#4971,#2570,.T.);
#6344=EDGE_CURVE('',#4971,#4955,#3323,.T.);
#6345=EDGE_CURVE('',#4972,#4973,#2571,.T.);
#6346=EDGE_CURVE('',#4974,#4974,#2572,.T.);
#6347=EDGE_CURVE('',#4975,#4975,#2573,.T.);
#6348=EDGE_CURVE('',#4975,#4974,#3324,.T.);
#6349=EDGE_CURVE('',#4976,#4977,#2574,.T.);
#6350=EDGE_CURVE('',#4977,#4976,#2575,.T.);
#6351=EDGE_CURVE('',#4976,#4975,#3325,.T.);
#6352=EDGE_CURVE('',#4978,#4978,#2576,.T.);
#6353=EDGE_CURVE('',#4979,#4979,#2577,.T.);
#6354=EDGE_CURVE('',#4980,#4981,#2578,.T.);
#6355=EDGE_CURVE('',#4981,#4980,#2579,.T.);
#6356=EDGE_CURVE('',#4980,#4979,#3326,.T.);
#6357=EDGE_CURVE('',#4977,#4978,#3327,.T.);
#6358=EDGE_CURVE('',#4981,#4982,#3328,.T.);
#6359=EDGE_CURVE('',#4982,#4982,#2580,.T.);
#6360=EDGE_CURVE('',#4983,#4983,#2581,.T.);
#6361=EDGE_CURVE('',#4983,#4984,#3329,.T.);
#6362=EDGE_CURVE('',#4984,#4984,#2582,.T.);
#6363=EDGE_CURVE('',#4984,#4985,#3330,.T.);
#6364=EDGE_CURVE('',#4985,#4985,#2583,.T.);
#6365=EDGE_CURVE('',#4986,#4986,#2584,.T.);
#6366=EDGE_CURVE('',#4986,#4986,#2585,.T.);
#6367=EDGE_CURVE('',#4987,#4988,#3331,.T.);
#6368=EDGE_CURVE('',#4987,#4989,#2586,.T.);
#6369=EDGE_CURVE('',#4990,#4989,#3332,.T.);
#6370=EDGE_CURVE('',#4990,#4991,#2587,.T.);
#6371=EDGE_CURVE('',#4992,#4991,#3333,.T.);
#6372=EDGE_CURVE('',#4992,#4993,#2588,.T.);
#6373=EDGE_CURVE('',#4994,#4993,#3334,.T.);
#6374=EDGE_CURVE('',#4994,#4995,#2589,.T.);
#6375=EDGE_CURVE('',#4996,#4995,#3335,.T.);
#6376=EDGE_CURVE('',#4996,#4997,#2590,.T.);
#6377=EDGE_CURVE('',#4998,#4997,#3336,.T.);
#6378=EDGE_CURVE('',#4998,#4988,#2591,.T.);
#6379=EDGE_CURVE('',#4999,#4999,#2592,.T.);
#6380=EDGE_CURVE('',#5000,#5001,#2593,.T.);
#6381=EDGE_CURVE('',#5000,#5002,#3337,.T.);
#6382=EDGE_CURVE('',#5003,#5002,#2594,.T.);
#6383=EDGE_CURVE('',#5003,#5004,#3338,.T.);
#6384=EDGE_CURVE('',#5005,#5004,#2595,.T.);
#6385=EDGE_CURVE('',#5005,#5006,#3339,.T.);
#6386=EDGE_CURVE('',#5007,#5006,#2596,.T.);
#6387=EDGE_CURVE('',#5007,#5008,#3340,.T.);
#6388=EDGE_CURVE('',#5009,#5008,#2597,.T.);
#6389=EDGE_CURVE('',#5009,#5010,#3341,.T.);
#6390=EDGE_CURVE('',#5011,#5010,#2598,.T.);
#6391=EDGE_CURVE('',#5011,#5001,#3342,.T.);
#6392=EDGE_CURVE('',#5012,#5012,#2599,.T.);
#6393=EDGE_CURVE('',#5013,#5014,#3343,.T.);
#6394=EDGE_CURVE('',#5014,#4996,#209,.T.);
#6395=EDGE_CURVE('',#4995,#5015,#210,.T.);
#6396=EDGE_CURVE('',#5016,#5015,#3344,.T.);
#6397=EDGE_CURVE('',#5016,#5006,#211,.T.);
#6398=EDGE_CURVE('',#5005,#5013,#212,.T.);
#6399=EDGE_CURVE('',#5015,#4994,#213,.T.);
#6400=EDGE_CURVE('',#4993,#5017,#214,.T.);
#6401=EDGE_CURVE('',#5018,#5017,#3345,.T.);
#6402=EDGE_CURVE('',#5018,#5008,#215,.T.);
#6403=EDGE_CURVE('',#5007,#5016,#216,.T.);
#6404=EDGE_CURVE('',#5017,#4992,#217,.T.);
#6405=EDGE_CURVE('',#4991,#5019,#218,.T.);
#6406=EDGE_CURVE('',#5020,#5019,#3346,.T.);
#6407=EDGE_CURVE('',#5020,#5010,#219,.T.);
#6408=EDGE_CURVE('',#5009,#5018,#220,.T.);
#6409=EDGE_CURVE('',#5019,#4990,#221,.T.);
#6410=EDGE_CURVE('',#4989,#5021,#222,.T.);
#6411=EDGE_CURVE('',#5022,#5021,#3347,.T.);
#6412=EDGE_CURVE('',#5022,#5001,#223,.T.);
#6413=EDGE_CURVE('',#5011,#5020,#224,.T.);
#6414=EDGE_CURVE('',#5021,#4987,#225,.T.);
#6415=EDGE_CURVE('',#4988,#5023,#226,.T.);
#6416=EDGE_CURVE('',#5024,#5023,#3348,.T.);
#6417=EDGE_CURVE('',#5024,#5002,#227,.T.);
#6418=EDGE_CURVE('',#5000,#5022,#228,.T.);
#6419=EDGE_CURVE('',#5023,#4998,#229,.T.);
#6420=EDGE_CURVE('',#4997,#5014,#230,.T.);
#6421=EDGE_CURVE('',#5013,#5004,#231,.T.);
#6422=EDGE_CURVE('',#5003,#5024,#232,.T.);
#6423=EDGE_CURVE('',#5012,#4999,#3349,.T.);
#6424=ORIENTED_EDGE('',*,*,#5025,.T.);
#6425=ORIENTED_EDGE('',*,*,#5026,.T.);
#6426=ORIENTED_EDGE('',*,*,#5027,.F.);
#6427=ORIENTED_EDGE('',*,*,#5028,.T.);
#6428=ORIENTED_EDGE('',*,*,#5029,.T.);
#6429=ORIENTED_EDGE('',*,*,#5030,.T.);
#6430=ORIENTED_EDGE('',*,*,#5031,.F.);
#6431=ORIENTED_EDGE('',*,*,#5032,.T.);
#6432=ORIENTED_EDGE('',*,*,#5033,.T.);
#6433=ORIENTED_EDGE('',*,*,#5034,.T.);
#6434=ORIENTED_EDGE('',*,*,#5035,.F.);
#6435=ORIENTED_EDGE('',*,*,#5036,.T.);
#6436=ORIENTED_EDGE('',*,*,#5037,.T.);
#6437=ORIENTED_EDGE('',*,*,#5038,.T.);
#6438=ORIENTED_EDGE('',*,*,#5039,.F.);
#6439=ORIENTED_EDGE('',*,*,#5040,.T.);
#6440=ORIENTED_EDGE('',*,*,#5041,.T.);
#6441=ORIENTED_EDGE('',*,*,#5042,.T.);
#6442=ORIENTED_EDGE('',*,*,#5043,.F.);
#6443=ORIENTED_EDGE('',*,*,#5044,.T.);
#6444=ORIENTED_EDGE('',*,*,#5045,.T.);
#6445=ORIENTED_EDGE('',*,*,#5046,.T.);
#6446=ORIENTED_EDGE('',*,*,#5047,.F.);
#6447=ORIENTED_EDGE('',*,*,#5048,.T.);
#6448=ORIENTED_EDGE('',*,*,#5049,.T.);
#6449=ORIENTED_EDGE('',*,*,#5050,.T.);
#6450=ORIENTED_EDGE('',*,*,#5051,.F.);
#6451=ORIENTED_EDGE('',*,*,#5052,.T.);
#6452=ORIENTED_EDGE('',*,*,#5053,.T.);
#6453=ORIENTED_EDGE('',*,*,#5054,.T.);
#6454=ORIENTED_EDGE('',*,*,#5055,.F.);
#6455=ORIENTED_EDGE('',*,*,#5056,.T.);
#6456=ORIENTED_EDGE('',*,*,#5057,.T.);
#6457=ORIENTED_EDGE('',*,*,#5058,.T.);
#6458=ORIENTED_EDGE('',*,*,#5059,.F.);
#6459=ORIENTED_EDGE('',*,*,#5060,.T.);
#6460=ORIENTED_EDGE('',*,*,#5061,.T.);
#6461=ORIENTED_EDGE('',*,*,#5062,.T.);
#6462=ORIENTED_EDGE('',*,*,#5063,.F.);
#6463=ORIENTED_EDGE('',*,*,#5064,.T.);
#6464=ORIENTED_EDGE('',*,*,#5065,.T.);
#6465=ORIENTED_EDGE('',*,*,#5066,.T.);
#6466=ORIENTED_EDGE('',*,*,#5067,.F.);
#6467=ORIENTED_EDGE('',*,*,#5068,.T.);
#6468=ORIENTED_EDGE('',*,*,#5069,.T.);
#6469=ORIENTED_EDGE('',*,*,#5070,.T.);
#6470=ORIENTED_EDGE('',*,*,#5071,.F.);
#6471=ORIENTED_EDGE('',*,*,#5072,.T.);
#6472=ORIENTED_EDGE('',*,*,#5073,.T.);
#6473=ORIENTED_EDGE('',*,*,#5074,.T.);
#6474=ORIENTED_EDGE('',*,*,#5075,.F.);
#6475=ORIENTED_EDGE('',*,*,#5076,.T.);
#6476=ORIENTED_EDGE('',*,*,#5077,.T.);
#6477=ORIENTED_EDGE('',*,*,#5078,.T.);
#6478=ORIENTED_EDGE('',*,*,#5079,.F.);
#6479=ORIENTED_EDGE('',*,*,#5080,.T.);
#6480=ORIENTED_EDGE('',*,*,#5081,.T.);
#6481=ORIENTED_EDGE('',*,*,#5082,.T.);
#6482=ORIENTED_EDGE('',*,*,#5083,.F.);
#6483=ORIENTED_EDGE('',*,*,#5084,.T.);
#6484=ORIENTED_EDGE('',*,*,#5085,.T.);
#6485=ORIENTED_EDGE('',*,*,#5086,.T.);
#6486=ORIENTED_EDGE('',*,*,#5087,.F.);
#6487=ORIENTED_EDGE('',*,*,#5088,.T.);
#6488=ORIENTED_EDGE('',*,*,#5089,.T.);
#6489=ORIENTED_EDGE('',*,*,#5090,.T.);
#6490=ORIENTED_EDGE('',*,*,#5091,.F.);
#6491=ORIENTED_EDGE('',*,*,#5092,.T.);
#6492=ORIENTED_EDGE('',*,*,#5093,.T.);
#6493=ORIENTED_EDGE('',*,*,#5094,.T.);
#6494=ORIENTED_EDGE('',*,*,#5095,.F.);
#6495=ORIENTED_EDGE('',*,*,#5096,.T.);
#6496=ORIENTED_EDGE('',*,*,#5097,.T.);
#6497=ORIENTED_EDGE('',*,*,#5098,.T.);
#6498=ORIENTED_EDGE('',*,*,#5099,.F.);
#6499=ORIENTED_EDGE('',*,*,#5100,.T.);
#6500=ORIENTED_EDGE('',*,*,#5101,.T.);
#6501=ORIENTED_EDGE('',*,*,#5102,.T.);
#6502=ORIENTED_EDGE('',*,*,#5103,.F.);
#6503=ORIENTED_EDGE('',*,*,#5104,.T.);
#6504=ORIENTED_EDGE('',*,*,#5105,.T.);
#6505=ORIENTED_EDGE('',*,*,#5106,.T.);
#6506=ORIENTED_EDGE('',*,*,#5107,.F.);
#6507=ORIENTED_EDGE('',*,*,#5108,.T.);
#6508=ORIENTED_EDGE('',*,*,#5109,.T.);
#6509=ORIENTED_EDGE('',*,*,#5110,.T.);
#6510=ORIENTED_EDGE('',*,*,#5111,.F.);
#6511=ORIENTED_EDGE('',*,*,#5112,.T.);
#6512=ORIENTED_EDGE('',*,*,#5113,.T.);
#6513=ORIENTED_EDGE('',*,*,#5114,.T.);
#6514=ORIENTED_EDGE('',*,*,#5115,.F.);
#6515=ORIENTED_EDGE('',*,*,#5116,.T.);
#6516=ORIENTED_EDGE('',*,*,#5117,.T.);
#6517=ORIENTED_EDGE('',*,*,#5118,.T.);
#6518=ORIENTED_EDGE('',*,*,#5119,.F.);
#6519=ORIENTED_EDGE('',*,*,#5120,.T.);
#6520=ORIENTED_EDGE('',*,*,#5121,.T.);
#6521=ORIENTED_EDGE('',*,*,#5122,.T.);
#6522=ORIENTED_EDGE('',*,*,#5123,.F.);
#6523=ORIENTED_EDGE('',*,*,#5124,.T.);
#6524=ORIENTED_EDGE('',*,*,#5125,.T.);
#6525=ORIENTED_EDGE('',*,*,#5126,.T.);
#6526=ORIENTED_EDGE('',*,*,#5127,.F.);
#6527=ORIENTED_EDGE('',*,*,#5128,.T.);
#6528=ORIENTED_EDGE('',*,*,#5129,.T.);
#6529=ORIENTED_EDGE('',*,*,#5130,.T.);
#6530=ORIENTED_EDGE('',*,*,#5131,.F.);
#6531=ORIENTED_EDGE('',*,*,#5132,.T.);
#6532=ORIENTED_EDGE('',*,*,#5133,.T.);
#6533=ORIENTED_EDGE('',*,*,#5134,.T.);
#6534=ORIENTED_EDGE('',*,*,#5135,.F.);
#6535=ORIENTED_EDGE('',*,*,#5136,.T.);
#6536=ORIENTED_EDGE('',*,*,#5137,.T.);
#6537=ORIENTED_EDGE('',*,*,#5138,.T.);
#6538=ORIENTED_EDGE('',*,*,#5139,.F.);
#6539=ORIENTED_EDGE('',*,*,#5140,.T.);
#6540=ORIENTED_EDGE('',*,*,#5141,.T.);
#6541=ORIENTED_EDGE('',*,*,#5142,.T.);
#6542=ORIENTED_EDGE('',*,*,#5143,.F.);
#6543=ORIENTED_EDGE('',*,*,#5144,.T.);
#6544=ORIENTED_EDGE('',*,*,#5145,.T.);
#6545=ORIENTED_EDGE('',*,*,#5146,.T.);
#6546=ORIENTED_EDGE('',*,*,#5147,.F.);
#6547=ORIENTED_EDGE('',*,*,#5148,.T.);
#6548=ORIENTED_EDGE('',*,*,#5149,.T.);
#6549=ORIENTED_EDGE('',*,*,#5150,.T.);
#6550=ORIENTED_EDGE('',*,*,#5151,.F.);
#6551=ORIENTED_EDGE('',*,*,#5152,.T.);
#6552=ORIENTED_EDGE('',*,*,#5153,.T.);
#6553=ORIENTED_EDGE('',*,*,#5154,.T.);
#6554=ORIENTED_EDGE('',*,*,#5155,.F.);
#6555=ORIENTED_EDGE('',*,*,#5156,.T.);
#6556=ORIENTED_EDGE('',*,*,#5157,.T.);
#6557=ORIENTED_EDGE('',*,*,#5158,.T.);
#6558=ORIENTED_EDGE('',*,*,#5159,.F.);
#6559=ORIENTED_EDGE('',*,*,#5160,.T.);
#6560=ORIENTED_EDGE('',*,*,#5161,.T.);
#6561=ORIENTED_EDGE('',*,*,#5162,.T.);
#6562=ORIENTED_EDGE('',*,*,#5163,.F.);
#6563=ORIENTED_EDGE('',*,*,#5164,.T.);
#6564=ORIENTED_EDGE('',*,*,#5165,.T.);
#6565=ORIENTED_EDGE('',*,*,#5166,.T.);
#6566=ORIENTED_EDGE('',*,*,#5167,.F.);
#6567=ORIENTED_EDGE('',*,*,#5168,.T.);
#6568=ORIENTED_EDGE('',*,*,#5169,.T.);
#6569=ORIENTED_EDGE('',*,*,#5170,.T.);
#6570=ORIENTED_EDGE('',*,*,#5171,.F.);
#6571=ORIENTED_EDGE('',*,*,#5172,.T.);
#6572=ORIENTED_EDGE('',*,*,#5173,.T.);
#6573=ORIENTED_EDGE('',*,*,#5174,.T.);
#6574=ORIENTED_EDGE('',*,*,#5175,.F.);
#6575=ORIENTED_EDGE('',*,*,#5176,.T.);
#6576=ORIENTED_EDGE('',*,*,#5177,.T.);
#6577=ORIENTED_EDGE('',*,*,#5178,.T.);
#6578=ORIENTED_EDGE('',*,*,#5179,.F.);
#6579=ORIENTED_EDGE('',*,*,#5180,.T.);
#6580=ORIENTED_EDGE('',*,*,#5181,.T.);
#6581=ORIENTED_EDGE('',*,*,#5182,.T.);
#6582=ORIENTED_EDGE('',*,*,#5183,.F.);
#6583=ORIENTED_EDGE('',*,*,#5184,.T.);
#6584=ORIENTED_EDGE('',*,*,#5185,.F.);
#6585=ORIENTED_EDGE('',*,*,#5186,.F.);
#6586=ORIENTED_EDGE('',*,*,#5187,.T.);
#6587=ORIENTED_EDGE('',*,*,#5179,.T.);
#6588=ORIENTED_EDGE('',*,*,#5188,.F.);
#6589=ORIENTED_EDGE('',*,*,#5181,.F.);
#6590=ORIENTED_EDGE('',*,*,#5189,.T.);
#6591=ORIENTED_EDGE('',*,*,#5186,.T.);
#6592=ORIENTED_EDGE('',*,*,#5190,.F.);
#6593=ORIENTED_EDGE('',*,*,#5191,.F.);
#6594=ORIENTED_EDGE('',*,*,#5192,.T.);
#6595=ORIENTED_EDGE('',*,*,#5175,.T.);
#6596=ORIENTED_EDGE('',*,*,#5193,.F.);
#6597=ORIENTED_EDGE('',*,*,#5177,.F.);
#6598=ORIENTED_EDGE('',*,*,#5194,.T.);
#6599=ORIENTED_EDGE('',*,*,#5191,.T.);
#6600=ORIENTED_EDGE('',*,*,#5195,.F.);
#6601=ORIENTED_EDGE('',*,*,#5196,.F.);
#6602=ORIENTED_EDGE('',*,*,#5197,.T.);
#6603=ORIENTED_EDGE('',*,*,#5171,.T.);
#6604=ORIENTED_EDGE('',*,*,#5198,.F.);
#6605=ORIENTED_EDGE('',*,*,#5173,.F.);
#6606=ORIENTED_EDGE('',*,*,#5199,.T.);
#6607=ORIENTED_EDGE('',*,*,#5196,.T.);
#6608=ORIENTED_EDGE('',*,*,#5200,.F.);
#6609=ORIENTED_EDGE('',*,*,#5201,.F.);
#6610=ORIENTED_EDGE('',*,*,#5202,.T.);
#6611=ORIENTED_EDGE('',*,*,#5167,.T.);
#6612=ORIENTED_EDGE('',*,*,#5203,.F.);
#6613=ORIENTED_EDGE('',*,*,#5169,.F.);
#6614=ORIENTED_EDGE('',*,*,#5204,.T.);
#6615=ORIENTED_EDGE('',*,*,#5201,.T.);
#6616=ORIENTED_EDGE('',*,*,#5205,.F.);
#6617=ORIENTED_EDGE('',*,*,#5206,.F.);
#6618=ORIENTED_EDGE('',*,*,#5207,.T.);
#6619=ORIENTED_EDGE('',*,*,#5163,.T.);
#6620=ORIENTED_EDGE('',*,*,#5208,.F.);
#6621=ORIENTED_EDGE('',*,*,#5165,.F.);
#6622=ORIENTED_EDGE('',*,*,#5209,.T.);
#6623=ORIENTED_EDGE('',*,*,#5206,.T.);
#6624=ORIENTED_EDGE('',*,*,#5210,.F.);
#6625=ORIENTED_EDGE('',*,*,#5211,.F.);
#6626=ORIENTED_EDGE('',*,*,#5212,.T.);
#6627=ORIENTED_EDGE('',*,*,#5159,.T.);
#6628=ORIENTED_EDGE('',*,*,#5213,.F.);
#6629=ORIENTED_EDGE('',*,*,#5161,.F.);
#6630=ORIENTED_EDGE('',*,*,#5214,.T.);
#6631=ORIENTED_EDGE('',*,*,#5211,.T.);
#6632=ORIENTED_EDGE('',*,*,#5215,.F.);
#6633=ORIENTED_EDGE('',*,*,#5216,.F.);
#6634=ORIENTED_EDGE('',*,*,#5217,.T.);
#6635=ORIENTED_EDGE('',*,*,#5155,.T.);
#6636=ORIENTED_EDGE('',*,*,#5218,.F.);
#6637=ORIENTED_EDGE('',*,*,#5157,.F.);
#6638=ORIENTED_EDGE('',*,*,#5219,.T.);
#6639=ORIENTED_EDGE('',*,*,#5216,.T.);
#6640=ORIENTED_EDGE('',*,*,#5220,.F.);
#6641=ORIENTED_EDGE('',*,*,#5221,.F.);
#6642=ORIENTED_EDGE('',*,*,#5222,.T.);
#6643=ORIENTED_EDGE('',*,*,#5151,.T.);
#6644=ORIENTED_EDGE('',*,*,#5223,.F.);
#6645=ORIENTED_EDGE('',*,*,#5153,.F.);
#6646=ORIENTED_EDGE('',*,*,#5224,.T.);
#6647=ORIENTED_EDGE('',*,*,#5221,.T.);
#6648=ORIENTED_EDGE('',*,*,#5225,.F.);
#6649=ORIENTED_EDGE('',*,*,#5226,.F.);
#6650=ORIENTED_EDGE('',*,*,#5227,.T.);
#6651=ORIENTED_EDGE('',*,*,#5147,.T.);
#6652=ORIENTED_EDGE('',*,*,#5228,.F.);
#6653=ORIENTED_EDGE('',*,*,#5149,.F.);
#6654=ORIENTED_EDGE('',*,*,#5229,.T.);
#6655=ORIENTED_EDGE('',*,*,#5226,.T.);
#6656=ORIENTED_EDGE('',*,*,#5230,.F.);
#6657=ORIENTED_EDGE('',*,*,#5231,.F.);
#6658=ORIENTED_EDGE('',*,*,#5232,.T.);
#6659=ORIENTED_EDGE('',*,*,#5143,.T.);
#6660=ORIENTED_EDGE('',*,*,#5233,.F.);
#6661=ORIENTED_EDGE('',*,*,#5145,.F.);
#6662=ORIENTED_EDGE('',*,*,#5234,.T.);
#6663=ORIENTED_EDGE('',*,*,#5231,.T.);
#6664=ORIENTED_EDGE('',*,*,#5235,.F.);
#6665=ORIENTED_EDGE('',*,*,#5236,.F.);
#6666=ORIENTED_EDGE('',*,*,#5237,.T.);
#6667=ORIENTED_EDGE('',*,*,#5139,.T.);
#6668=ORIENTED_EDGE('',*,*,#5238,.F.);
#6669=ORIENTED_EDGE('',*,*,#5141,.F.);
#6670=ORIENTED_EDGE('',*,*,#5239,.T.);
#6671=ORIENTED_EDGE('',*,*,#5236,.T.);
#6672=ORIENTED_EDGE('',*,*,#5240,.F.);
#6673=ORIENTED_EDGE('',*,*,#5241,.F.);
#6674=ORIENTED_EDGE('',*,*,#5242,.T.);
#6675=ORIENTED_EDGE('',*,*,#5135,.T.);
#6676=ORIENTED_EDGE('',*,*,#5243,.F.);
#6677=ORIENTED_EDGE('',*,*,#5137,.F.);
#6678=ORIENTED_EDGE('',*,*,#5244,.T.);
#6679=ORIENTED_EDGE('',*,*,#5241,.T.);
#6680=ORIENTED_EDGE('',*,*,#5245,.F.);
#6681=ORIENTED_EDGE('',*,*,#5246,.F.);
#6682=ORIENTED_EDGE('',*,*,#5247,.T.);
#6683=ORIENTED_EDGE('',*,*,#5131,.T.);
#6684=ORIENTED_EDGE('',*,*,#5248,.F.);
#6685=ORIENTED_EDGE('',*,*,#5133,.F.);
#6686=ORIENTED_EDGE('',*,*,#5249,.T.);
#6687=ORIENTED_EDGE('',*,*,#5246,.T.);
#6688=ORIENTED_EDGE('',*,*,#5250,.F.);
#6689=ORIENTED_EDGE('',*,*,#5251,.F.);
#6690=ORIENTED_EDGE('',*,*,#5252,.T.);
#6691=ORIENTED_EDGE('',*,*,#5127,.T.);
#6692=ORIENTED_EDGE('',*,*,#5253,.F.);
#6693=ORIENTED_EDGE('',*,*,#5129,.F.);
#6694=ORIENTED_EDGE('',*,*,#5254,.T.);
#6695=ORIENTED_EDGE('',*,*,#5251,.T.);
#6696=ORIENTED_EDGE('',*,*,#5255,.F.);
#6697=ORIENTED_EDGE('',*,*,#5256,.F.);
#6698=ORIENTED_EDGE('',*,*,#5257,.T.);
#6699=ORIENTED_EDGE('',*,*,#5123,.T.);
#6700=ORIENTED_EDGE('',*,*,#5258,.F.);
#6701=ORIENTED_EDGE('',*,*,#5125,.F.);
#6702=ORIENTED_EDGE('',*,*,#5259,.T.);
#6703=ORIENTED_EDGE('',*,*,#5256,.T.);
#6704=ORIENTED_EDGE('',*,*,#5260,.F.);
#6705=ORIENTED_EDGE('',*,*,#5261,.F.);
#6706=ORIENTED_EDGE('',*,*,#5262,.T.);
#6707=ORIENTED_EDGE('',*,*,#5119,.T.);
#6708=ORIENTED_EDGE('',*,*,#5263,.F.);
#6709=ORIENTED_EDGE('',*,*,#5121,.F.);
#6710=ORIENTED_EDGE('',*,*,#5264,.T.);
#6711=ORIENTED_EDGE('',*,*,#5261,.T.);
#6712=ORIENTED_EDGE('',*,*,#5265,.F.);
#6713=ORIENTED_EDGE('',*,*,#5266,.F.);
#6714=ORIENTED_EDGE('',*,*,#5267,.T.);
#6715=ORIENTED_EDGE('',*,*,#5115,.T.);
#6716=ORIENTED_EDGE('',*,*,#5268,.F.);
#6717=ORIENTED_EDGE('',*,*,#5117,.F.);
#6718=ORIENTED_EDGE('',*,*,#5269,.T.);
#6719=ORIENTED_EDGE('',*,*,#5266,.T.);
#6720=ORIENTED_EDGE('',*,*,#5270,.F.);
#6721=ORIENTED_EDGE('',*,*,#5271,.F.);
#6722=ORIENTED_EDGE('',*,*,#5272,.T.);
#6723=ORIENTED_EDGE('',*,*,#5111,.T.);
#6724=ORIENTED_EDGE('',*,*,#5273,.F.);
#6725=ORIENTED_EDGE('',*,*,#5113,.F.);
#6726=ORIENTED_EDGE('',*,*,#5274,.T.);
#6727=ORIENTED_EDGE('',*,*,#5271,.T.);
#6728=ORIENTED_EDGE('',*,*,#5275,.F.);
#6729=ORIENTED_EDGE('',*,*,#5276,.F.);
#6730=ORIENTED_EDGE('',*,*,#5277,.T.);
#6731=ORIENTED_EDGE('',*,*,#5107,.T.);
#6732=ORIENTED_EDGE('',*,*,#5278,.F.);
#6733=ORIENTED_EDGE('',*,*,#5109,.F.);
#6734=ORIENTED_EDGE('',*,*,#5279,.T.);
#6735=ORIENTED_EDGE('',*,*,#5276,.T.);
#6736=ORIENTED_EDGE('',*,*,#5280,.F.);
#6737=ORIENTED_EDGE('',*,*,#5281,.F.);
#6738=ORIENTED_EDGE('',*,*,#5282,.T.);
#6739=ORIENTED_EDGE('',*,*,#5103,.T.);
#6740=ORIENTED_EDGE('',*,*,#5283,.F.);
#6741=ORIENTED_EDGE('',*,*,#5105,.F.);
#6742=ORIENTED_EDGE('',*,*,#5284,.T.);
#6743=ORIENTED_EDGE('',*,*,#5281,.T.);
#6744=ORIENTED_EDGE('',*,*,#5285,.F.);
#6745=ORIENTED_EDGE('',*,*,#5286,.F.);
#6746=ORIENTED_EDGE('',*,*,#5287,.T.);
#6747=ORIENTED_EDGE('',*,*,#5099,.T.);
#6748=ORIENTED_EDGE('',*,*,#5288,.F.);
#6749=ORIENTED_EDGE('',*,*,#5101,.F.);
#6750=ORIENTED_EDGE('',*,*,#5289,.T.);
#6751=ORIENTED_EDGE('',*,*,#5286,.T.);
#6752=ORIENTED_EDGE('',*,*,#5290,.F.);
#6753=ORIENTED_EDGE('',*,*,#5291,.F.);
#6754=ORIENTED_EDGE('',*,*,#5292,.T.);
#6755=ORIENTED_EDGE('',*,*,#5095,.T.);
#6756=ORIENTED_EDGE('',*,*,#5293,.F.);
#6757=ORIENTED_EDGE('',*,*,#5097,.F.);
#6758=ORIENTED_EDGE('',*,*,#5294,.T.);
#6759=ORIENTED_EDGE('',*,*,#5291,.T.);
#6760=ORIENTED_EDGE('',*,*,#5295,.F.);
#6761=ORIENTED_EDGE('',*,*,#5296,.F.);
#6762=ORIENTED_EDGE('',*,*,#5297,.T.);
#6763=ORIENTED_EDGE('',*,*,#5091,.T.);
#6764=ORIENTED_EDGE('',*,*,#5298,.F.);
#6765=ORIENTED_EDGE('',*,*,#5093,.F.);
#6766=ORIENTED_EDGE('',*,*,#5299,.T.);
#6767=ORIENTED_EDGE('',*,*,#5296,.T.);
#6768=ORIENTED_EDGE('',*,*,#5300,.F.);
#6769=ORIENTED_EDGE('',*,*,#5301,.F.);
#6770=ORIENTED_EDGE('',*,*,#5302,.T.);
#6771=ORIENTED_EDGE('',*,*,#5087,.T.);
#6772=ORIENTED_EDGE('',*,*,#5303,.F.);
#6773=ORIENTED_EDGE('',*,*,#5089,.F.);
#6774=ORIENTED_EDGE('',*,*,#5304,.T.);
#6775=ORIENTED_EDGE('',*,*,#5301,.T.);
#6776=ORIENTED_EDGE('',*,*,#5305,.F.);
#6777=ORIENTED_EDGE('',*,*,#5306,.F.);
#6778=ORIENTED_EDGE('',*,*,#5307,.T.);
#6779=ORIENTED_EDGE('',*,*,#5083,.T.);
#6780=ORIENTED_EDGE('',*,*,#5308,.F.);
#6781=ORIENTED_EDGE('',*,*,#5085,.F.);
#6782=ORIENTED_EDGE('',*,*,#5309,.T.);
#6783=ORIENTED_EDGE('',*,*,#5306,.T.);
#6784=ORIENTED_EDGE('',*,*,#5310,.F.);
#6785=ORIENTED_EDGE('',*,*,#5311,.F.);
#6786=ORIENTED_EDGE('',*,*,#5312,.T.);
#6787=ORIENTED_EDGE('',*,*,#5079,.T.);
#6788=ORIENTED_EDGE('',*,*,#5313,.F.);
#6789=ORIENTED_EDGE('',*,*,#5081,.F.);
#6790=ORIENTED_EDGE('',*,*,#5314,.T.);
#6791=ORIENTED_EDGE('',*,*,#5311,.T.);
#6792=ORIENTED_EDGE('',*,*,#5315,.F.);
#6793=ORIENTED_EDGE('',*,*,#5316,.F.);
#6794=ORIENTED_EDGE('',*,*,#5317,.T.);
#6795=ORIENTED_EDGE('',*,*,#5075,.T.);
#6796=ORIENTED_EDGE('',*,*,#5318,.F.);
#6797=ORIENTED_EDGE('',*,*,#5077,.F.);
#6798=ORIENTED_EDGE('',*,*,#5319,.T.);
#6799=ORIENTED_EDGE('',*,*,#5316,.T.);
#6800=ORIENTED_EDGE('',*,*,#5320,.F.);
#6801=ORIENTED_EDGE('',*,*,#5321,.F.);
#6802=ORIENTED_EDGE('',*,*,#5322,.T.);
#6803=ORIENTED_EDGE('',*,*,#5071,.T.);
#6804=ORIENTED_EDGE('',*,*,#5323,.F.);
#6805=ORIENTED_EDGE('',*,*,#5073,.F.);
#6806=ORIENTED_EDGE('',*,*,#5324,.T.);
#6807=ORIENTED_EDGE('',*,*,#5321,.T.);
#6808=ORIENTED_EDGE('',*,*,#5325,.F.);
#6809=ORIENTED_EDGE('',*,*,#5326,.F.);
#6810=ORIENTED_EDGE('',*,*,#5327,.T.);
#6811=ORIENTED_EDGE('',*,*,#5067,.T.);
#6812=ORIENTED_EDGE('',*,*,#5328,.F.);
#6813=ORIENTED_EDGE('',*,*,#5069,.F.);
#6814=ORIENTED_EDGE('',*,*,#5329,.T.);
#6815=ORIENTED_EDGE('',*,*,#5326,.T.);
#6816=ORIENTED_EDGE('',*,*,#5330,.F.);
#6817=ORIENTED_EDGE('',*,*,#5331,.F.);
#6818=ORIENTED_EDGE('',*,*,#5332,.T.);
#6819=ORIENTED_EDGE('',*,*,#5063,.T.);
#6820=ORIENTED_EDGE('',*,*,#5333,.F.);
#6821=ORIENTED_EDGE('',*,*,#5065,.F.);
#6822=ORIENTED_EDGE('',*,*,#5334,.T.);
#6823=ORIENTED_EDGE('',*,*,#5331,.T.);
#6824=ORIENTED_EDGE('',*,*,#5335,.F.);
#6825=ORIENTED_EDGE('',*,*,#5336,.F.);
#6826=ORIENTED_EDGE('',*,*,#5337,.T.);
#6827=ORIENTED_EDGE('',*,*,#5059,.T.);
#6828=ORIENTED_EDGE('',*,*,#5338,.F.);
#6829=ORIENTED_EDGE('',*,*,#5061,.F.);
#6830=ORIENTED_EDGE('',*,*,#5339,.T.);
#6831=ORIENTED_EDGE('',*,*,#5336,.T.);
#6832=ORIENTED_EDGE('',*,*,#5340,.F.);
#6833=ORIENTED_EDGE('',*,*,#5341,.F.);
#6834=ORIENTED_EDGE('',*,*,#5342,.T.);
#6835=ORIENTED_EDGE('',*,*,#5055,.T.);
#6836=ORIENTED_EDGE('',*,*,#5343,.F.);
#6837=ORIENTED_EDGE('',*,*,#5057,.F.);
#6838=ORIENTED_EDGE('',*,*,#5344,.T.);
#6839=ORIENTED_EDGE('',*,*,#5341,.T.);
#6840=ORIENTED_EDGE('',*,*,#5345,.F.);
#6841=ORIENTED_EDGE('',*,*,#5346,.F.);
#6842=ORIENTED_EDGE('',*,*,#5347,.T.);
#6843=ORIENTED_EDGE('',*,*,#5051,.T.);
#6844=ORIENTED_EDGE('',*,*,#5348,.F.);
#6845=ORIENTED_EDGE('',*,*,#5053,.F.);
#6846=ORIENTED_EDGE('',*,*,#5349,.T.);
#6847=ORIENTED_EDGE('',*,*,#5346,.T.);
#6848=ORIENTED_EDGE('',*,*,#5350,.F.);
#6849=ORIENTED_EDGE('',*,*,#5351,.F.);
#6850=ORIENTED_EDGE('',*,*,#5352,.T.);
#6851=ORIENTED_EDGE('',*,*,#5047,.T.);
#6852=ORIENTED_EDGE('',*,*,#5353,.F.);
#6853=ORIENTED_EDGE('',*,*,#5049,.F.);
#6854=ORIENTED_EDGE('',*,*,#5354,.T.);
#6855=ORIENTED_EDGE('',*,*,#5351,.T.);
#6856=ORIENTED_EDGE('',*,*,#5355,.F.);
#6857=ORIENTED_EDGE('',*,*,#5356,.F.);
#6858=ORIENTED_EDGE('',*,*,#5357,.T.);
#6859=ORIENTED_EDGE('',*,*,#5043,.T.);
#6860=ORIENTED_EDGE('',*,*,#5358,.F.);
#6861=ORIENTED_EDGE('',*,*,#5045,.F.);
#6862=ORIENTED_EDGE('',*,*,#5359,.T.);
#6863=ORIENTED_EDGE('',*,*,#5356,.T.);
#6864=ORIENTED_EDGE('',*,*,#5360,.F.);
#6865=ORIENTED_EDGE('',*,*,#5361,.F.);
#6866=ORIENTED_EDGE('',*,*,#5362,.T.);
#6867=ORIENTED_EDGE('',*,*,#5039,.T.);
#6868=ORIENTED_EDGE('',*,*,#5363,.F.);
#6869=ORIENTED_EDGE('',*,*,#5041,.F.);
#6870=ORIENTED_EDGE('',*,*,#5364,.T.);
#6871=ORIENTED_EDGE('',*,*,#5361,.T.);
#6872=ORIENTED_EDGE('',*,*,#5365,.F.);
#6873=ORIENTED_EDGE('',*,*,#5366,.F.);
#6874=ORIENTED_EDGE('',*,*,#5367,.T.);
#6875=ORIENTED_EDGE('',*,*,#5035,.T.);
#6876=ORIENTED_EDGE('',*,*,#5368,.F.);
#6877=ORIENTED_EDGE('',*,*,#5037,.F.);
#6878=ORIENTED_EDGE('',*,*,#5369,.T.);
#6879=ORIENTED_EDGE('',*,*,#5366,.T.);
#6880=ORIENTED_EDGE('',*,*,#5370,.F.);
#6881=ORIENTED_EDGE('',*,*,#5371,.F.);
#6882=ORIENTED_EDGE('',*,*,#5372,.T.);
#6883=ORIENTED_EDGE('',*,*,#5031,.T.);
#6884=ORIENTED_EDGE('',*,*,#5373,.F.);
#6885=ORIENTED_EDGE('',*,*,#5033,.F.);
#6886=ORIENTED_EDGE('',*,*,#5374,.T.);
#6887=ORIENTED_EDGE('',*,*,#5371,.T.);
#6888=ORIENTED_EDGE('',*,*,#5375,.F.);
#6889=ORIENTED_EDGE('',*,*,#5376,.F.);
#6890=ORIENTED_EDGE('',*,*,#5377,.T.);
#6891=ORIENTED_EDGE('',*,*,#5027,.T.);
#6892=ORIENTED_EDGE('',*,*,#5378,.F.);
#6893=ORIENTED_EDGE('',*,*,#5029,.F.);
#6894=ORIENTED_EDGE('',*,*,#5379,.T.);
#6895=ORIENTED_EDGE('',*,*,#5376,.T.);
#6896=ORIENTED_EDGE('',*,*,#5380,.F.);
#6897=ORIENTED_EDGE('',*,*,#5381,.F.);
#6898=ORIENTED_EDGE('',*,*,#5382,.T.);
#6899=ORIENTED_EDGE('',*,*,#5183,.T.);
#6900=ORIENTED_EDGE('',*,*,#5383,.F.);
#6901=ORIENTED_EDGE('',*,*,#5025,.F.);
#6902=ORIENTED_EDGE('',*,*,#5384,.T.);
#6903=ORIENTED_EDGE('',*,*,#5381,.T.);
#6904=ORIENTED_EDGE('',*,*,#5385,.T.);
#6905=ORIENTED_EDGE('',*,*,#5386,.T.);
#6906=ORIENTED_EDGE('',*,*,#5387,.T.);
#6907=ORIENTED_EDGE('',*,*,#5388,.T.);
#6908=ORIENTED_EDGE('',*,*,#5389,.T.);
#6909=ORIENTED_EDGE('',*,*,#5390,.T.);
#6910=ORIENTED_EDGE('',*,*,#5391,.T.);
#6911=ORIENTED_EDGE('',*,*,#5392,.T.);
#6912=ORIENTED_EDGE('',*,*,#5393,.T.);
#6913=ORIENTED_EDGE('',*,*,#5382,.F.);
#6914=ORIENTED_EDGE('',*,*,#5384,.F.);
#6915=ORIENTED_EDGE('',*,*,#5028,.F.);
#6916=ORIENTED_EDGE('',*,*,#5377,.F.);
#6917=ORIENTED_EDGE('',*,*,#5379,.F.);
#6918=ORIENTED_EDGE('',*,*,#5032,.F.);
#6919=ORIENTED_EDGE('',*,*,#5372,.F.);
#6920=ORIENTED_EDGE('',*,*,#5374,.F.);
#6921=ORIENTED_EDGE('',*,*,#5036,.F.);
#6922=ORIENTED_EDGE('',*,*,#5367,.F.);
#6923=ORIENTED_EDGE('',*,*,#5369,.F.);
#6924=ORIENTED_EDGE('',*,*,#5040,.F.);
#6925=ORIENTED_EDGE('',*,*,#5362,.F.);
#6926=ORIENTED_EDGE('',*,*,#5364,.F.);
#6927=ORIENTED_EDGE('',*,*,#5044,.F.);
#6928=ORIENTED_EDGE('',*,*,#5357,.F.);
#6929=ORIENTED_EDGE('',*,*,#5359,.F.);
#6930=ORIENTED_EDGE('',*,*,#5048,.F.);
#6931=ORIENTED_EDGE('',*,*,#5352,.F.);
#6932=ORIENTED_EDGE('',*,*,#5354,.F.);
#6933=ORIENTED_EDGE('',*,*,#5052,.F.);
#6934=ORIENTED_EDGE('',*,*,#5347,.F.);
#6935=ORIENTED_EDGE('',*,*,#5349,.F.);
#6936=ORIENTED_EDGE('',*,*,#5056,.F.);
#6937=ORIENTED_EDGE('',*,*,#5342,.F.);
#6938=ORIENTED_EDGE('',*,*,#5344,.F.);
#6939=ORIENTED_EDGE('',*,*,#5060,.F.);
#6940=ORIENTED_EDGE('',*,*,#5337,.F.);
#6941=ORIENTED_EDGE('',*,*,#5339,.F.);
#6942=ORIENTED_EDGE('',*,*,#5064,.F.);
#6943=ORIENTED_EDGE('',*,*,#5332,.F.);
#6944=ORIENTED_EDGE('',*,*,#5334,.F.);
#6945=ORIENTED_EDGE('',*,*,#5068,.F.);
#6946=ORIENTED_EDGE('',*,*,#5327,.F.);
#6947=ORIENTED_EDGE('',*,*,#5329,.F.);
#6948=ORIENTED_EDGE('',*,*,#5072,.F.);
#6949=ORIENTED_EDGE('',*,*,#5322,.F.);
#6950=ORIENTED_EDGE('',*,*,#5324,.F.);
#6951=ORIENTED_EDGE('',*,*,#5076,.F.);
#6952=ORIENTED_EDGE('',*,*,#5317,.F.);
#6953=ORIENTED_EDGE('',*,*,#5319,.F.);
#6954=ORIENTED_EDGE('',*,*,#5080,.F.);
#6955=ORIENTED_EDGE('',*,*,#5312,.F.);
#6956=ORIENTED_EDGE('',*,*,#5314,.F.);
#6957=ORIENTED_EDGE('',*,*,#5084,.F.);
#6958=ORIENTED_EDGE('',*,*,#5307,.F.);
#6959=ORIENTED_EDGE('',*,*,#5309,.F.);
#6960=ORIENTED_EDGE('',*,*,#5088,.F.);
#6961=ORIENTED_EDGE('',*,*,#5302,.F.);
#6962=ORIENTED_EDGE('',*,*,#5304,.F.);
#6963=ORIENTED_EDGE('',*,*,#5092,.F.);
#6964=ORIENTED_EDGE('',*,*,#5297,.F.);
#6965=ORIENTED_EDGE('',*,*,#5299,.F.);
#6966=ORIENTED_EDGE('',*,*,#5096,.F.);
#6967=ORIENTED_EDGE('',*,*,#5292,.F.);
#6968=ORIENTED_EDGE('',*,*,#5294,.F.);
#6969=ORIENTED_EDGE('',*,*,#5100,.F.);
#6970=ORIENTED_EDGE('',*,*,#5287,.F.);
#6971=ORIENTED_EDGE('',*,*,#5289,.F.);
#6972=ORIENTED_EDGE('',*,*,#5104,.F.);
#6973=ORIENTED_EDGE('',*,*,#5282,.F.);
#6974=ORIENTED_EDGE('',*,*,#5284,.F.);
#6975=ORIENTED_EDGE('',*,*,#5108,.F.);
#6976=ORIENTED_EDGE('',*,*,#5277,.F.);
#6977=ORIENTED_EDGE('',*,*,#5279,.F.);
#6978=ORIENTED_EDGE('',*,*,#5112,.F.);
#6979=ORIENTED_EDGE('',*,*,#5272,.F.);
#6980=ORIENTED_EDGE('',*,*,#5274,.F.);
#6981=ORIENTED_EDGE('',*,*,#5116,.F.);
#6982=ORIENTED_EDGE('',*,*,#5267,.F.);
#6983=ORIENTED_EDGE('',*,*,#5269,.F.);
#6984=ORIENTED_EDGE('',*,*,#5120,.F.);
#6985=ORIENTED_EDGE('',*,*,#5262,.F.);
#6986=ORIENTED_EDGE('',*,*,#5264,.F.);
#6987=ORIENTED_EDGE('',*,*,#5124,.F.);
#6988=ORIENTED_EDGE('',*,*,#5257,.F.);
#6989=ORIENTED_EDGE('',*,*,#5259,.F.);
#6990=ORIENTED_EDGE('',*,*,#5128,.F.);
#6991=ORIENTED_EDGE('',*,*,#5252,.F.);
#6992=ORIENTED_EDGE('',*,*,#5254,.F.);
#6993=ORIENTED_EDGE('',*,*,#5132,.F.);
#6994=ORIENTED_EDGE('',*,*,#5247,.F.);
#6995=ORIENTED_EDGE('',*,*,#5249,.F.);
#6996=ORIENTED_EDGE('',*,*,#5136,.F.);
#6997=ORIENTED_EDGE('',*,*,#5242,.F.);
#6998=ORIENTED_EDGE('',*,*,#5244,.F.);
#6999=ORIENTED_EDGE('',*,*,#5140,.F.);
#7000=ORIENTED_EDGE('',*,*,#5237,.F.);
#7001=ORIENTED_EDGE('',*,*,#5239,.F.);
#7002=ORIENTED_EDGE('',*,*,#5144,.F.);
#7003=ORIENTED_EDGE('',*,*,#5232,.F.);
#7004=ORIENTED_EDGE('',*,*,#5234,.F.);
#7005=ORIENTED_EDGE('',*,*,#5148,.F.);
#7006=ORIENTED_EDGE('',*,*,#5227,.F.);
#7007=ORIENTED_EDGE('',*,*,#5229,.F.);
#7008=ORIENTED_EDGE('',*,*,#5152,.F.);
#7009=ORIENTED_EDGE('',*,*,#5222,.F.);
#7010=ORIENTED_EDGE('',*,*,#5224,.F.);
#7011=ORIENTED_EDGE('',*,*,#5156,.F.);
#7012=ORIENTED_EDGE('',*,*,#5217,.F.);
#7013=ORIENTED_EDGE('',*,*,#5219,.F.);
#7014=ORIENTED_EDGE('',*,*,#5160,.F.);
#7015=ORIENTED_EDGE('',*,*,#5212,.F.);
#7016=ORIENTED_EDGE('',*,*,#5214,.F.);
#7017=ORIENTED_EDGE('',*,*,#5164,.F.);
#7018=ORIENTED_EDGE('',*,*,#5207,.F.);
#7019=ORIENTED_EDGE('',*,*,#5209,.F.);
#7020=ORIENTED_EDGE('',*,*,#5168,.F.);
#7021=ORIENTED_EDGE('',*,*,#5202,.F.);
#7022=ORIENTED_EDGE('',*,*,#5204,.F.);
#7023=ORIENTED_EDGE('',*,*,#5172,.F.);
#7024=ORIENTED_EDGE('',*,*,#5197,.F.);
#7025=ORIENTED_EDGE('',*,*,#5199,.F.);
#7026=ORIENTED_EDGE('',*,*,#5176,.F.);
#7027=ORIENTED_EDGE('',*,*,#5192,.F.);
#7028=ORIENTED_EDGE('',*,*,#5194,.F.);
#7029=ORIENTED_EDGE('',*,*,#5180,.F.);
#7030=ORIENTED_EDGE('',*,*,#5187,.F.);
#7031=ORIENTED_EDGE('',*,*,#5189,.F.);
#7032=ORIENTED_EDGE('',*,*,#5184,.F.);
#7033=ORIENTED_EDGE('',*,*,#5394,.T.);
#7034=ORIENTED_EDGE('',*,*,#5395,.T.);
#7035=ORIENTED_EDGE('',*,*,#5396,.T.);
#7036=ORIENTED_EDGE('',*,*,#5397,.T.);
#7037=ORIENTED_EDGE('',*,*,#5398,.T.);
#7038=ORIENTED_EDGE('',*,*,#5399,.F.);
#7039=ORIENTED_EDGE('',*,*,#5400,.T.);
#7040=ORIENTED_EDGE('',*,*,#5401,.T.);
#7041=ORIENTED_EDGE('',*,*,#5402,.T.);
#7042=ORIENTED_EDGE('',*,*,#5403,.T.);
#7043=ORIENTED_EDGE('',*,*,#5404,.T.);
#7044=ORIENTED_EDGE('',*,*,#5405,.T.);
#7045=ORIENTED_EDGE('',*,*,#5406,.T.);
#7046=ORIENTED_EDGE('',*,*,#5407,.T.);
#7047=ORIENTED_EDGE('',*,*,#5408,.T.);
#7048=ORIENTED_EDGE('',*,*,#5401,.F.);
#7049=ORIENTED_EDGE('',*,*,#5409,.F.);
#7050=ORIENTED_EDGE('',*,*,#5410,.T.);
#7051=ORIENTED_EDGE('',*,*,#5406,.F.);
#7052=ORIENTED_EDGE('',*,*,#5411,.F.);
#7053=ORIENTED_EDGE('',*,*,#5412,.T.);
#7054=ORIENTED_EDGE('',*,*,#5385,.F.);
#7055=ORIENTED_EDGE('',*,*,#5413,.T.);
#7056=ORIENTED_EDGE('',*,*,#5409,.T.);
#7057=ORIENTED_EDGE('',*,*,#5405,.F.);
#7058=ORIENTED_EDGE('',*,*,#5404,.F.);
#7059=ORIENTED_EDGE('',*,*,#5414,.T.);
#7060=ORIENTED_EDGE('',*,*,#5411,.T.);
#7061=ORIENTED_EDGE('',*,*,#5407,.F.);
#7062=ORIENTED_EDGE('',*,*,#5415,.T.);
#7063=ORIENTED_EDGE('',*,*,#5416,.F.);
#7064=ORIENTED_EDGE('',*,*,#5416,.T.);
#7065=ORIENTED_EDGE('',*,*,#5417,.T.);
#7066=ORIENTED_EDGE('',*,*,#5387,.F.);
#7067=ORIENTED_EDGE('',*,*,#5418,.T.);
#7068=ORIENTED_EDGE('',*,*,#5419,.F.);
#7069=ORIENTED_EDGE('',*,*,#5402,.F.);
#7070=ORIENTED_EDGE('',*,*,#5408,.F.);
#7071=ORIENTED_EDGE('',*,*,#5419,.T.);
#7072=ORIENTED_EDGE('',*,*,#5420,.T.);
#7073=ORIENTED_EDGE('',*,*,#5403,.F.);
#7074=ORIENTED_EDGE('',*,*,#5421,.F.);
#7075=ORIENTED_EDGE('',*,*,#5422,.T.);
#7076=ORIENTED_EDGE('',*,*,#5399,.T.);
#7077=ORIENTED_EDGE('',*,*,#5422,.F.);
#7078=ORIENTED_EDGE('',*,*,#5421,.T.);
#7079=ORIENTED_EDGE('',*,*,#5318,.T.);
#7080=ORIENTED_EDGE('',*,*,#5315,.T.);
#7081=ORIENTED_EDGE('',*,*,#5074,.F.);
#7082=ORIENTED_EDGE('',*,*,#5323,.T.);
#7083=ORIENTED_EDGE('',*,*,#5320,.T.);
#7084=ORIENTED_EDGE('',*,*,#5070,.F.);
#7085=ORIENTED_EDGE('',*,*,#5328,.T.);
#7086=ORIENTED_EDGE('',*,*,#5325,.T.);
#7087=ORIENTED_EDGE('',*,*,#5066,.F.);
#7088=ORIENTED_EDGE('',*,*,#5333,.T.);
#7089=ORIENTED_EDGE('',*,*,#5330,.T.);
#7090=ORIENTED_EDGE('',*,*,#5062,.F.);
#7091=ORIENTED_EDGE('',*,*,#5338,.T.);
#7092=ORIENTED_EDGE('',*,*,#5335,.T.);
#7093=ORIENTED_EDGE('',*,*,#5058,.F.);
#7094=ORIENTED_EDGE('',*,*,#5343,.T.);
#7095=ORIENTED_EDGE('',*,*,#5340,.T.);
#7096=ORIENTED_EDGE('',*,*,#5054,.F.);
#7097=ORIENTED_EDGE('',*,*,#5348,.T.);
#7098=ORIENTED_EDGE('',*,*,#5345,.T.);
#7099=ORIENTED_EDGE('',*,*,#5050,.F.);
#7100=ORIENTED_EDGE('',*,*,#5353,.T.);
#7101=ORIENTED_EDGE('',*,*,#5350,.T.);
#7102=ORIENTED_EDGE('',*,*,#5046,.F.);
#7103=ORIENTED_EDGE('',*,*,#5358,.T.);
#7104=ORIENTED_EDGE('',*,*,#5355,.T.);
#7105=ORIENTED_EDGE('',*,*,#5042,.F.);
#7106=ORIENTED_EDGE('',*,*,#5363,.T.);
#7107=ORIENTED_EDGE('',*,*,#5360,.T.);
#7108=ORIENTED_EDGE('',*,*,#5038,.F.);
#7109=ORIENTED_EDGE('',*,*,#5368,.T.);
#7110=ORIENTED_EDGE('',*,*,#5365,.T.);
#7111=ORIENTED_EDGE('',*,*,#5034,.F.);
#7112=ORIENTED_EDGE('',*,*,#5373,.T.);
#7113=ORIENTED_EDGE('',*,*,#5370,.T.);
#7114=ORIENTED_EDGE('',*,*,#5030,.F.);
#7115=ORIENTED_EDGE('',*,*,#5378,.T.);
#7116=ORIENTED_EDGE('',*,*,#5375,.T.);
#7117=ORIENTED_EDGE('',*,*,#5026,.F.);
#7118=ORIENTED_EDGE('',*,*,#5383,.T.);
#7119=ORIENTED_EDGE('',*,*,#5380,.T.);
#7120=ORIENTED_EDGE('',*,*,#5182,.F.);
#7121=ORIENTED_EDGE('',*,*,#5188,.T.);
#7122=ORIENTED_EDGE('',*,*,#5185,.T.);
#7123=ORIENTED_EDGE('',*,*,#5178,.F.);
#7124=ORIENTED_EDGE('',*,*,#5193,.T.);
#7125=ORIENTED_EDGE('',*,*,#5190,.T.);
#7126=ORIENTED_EDGE('',*,*,#5174,.F.);
#7127=ORIENTED_EDGE('',*,*,#5198,.T.);
#7128=ORIENTED_EDGE('',*,*,#5195,.T.);
#7129=ORIENTED_EDGE('',*,*,#5170,.F.);
#7130=ORIENTED_EDGE('',*,*,#5203,.T.);
#7131=ORIENTED_EDGE('',*,*,#5200,.T.);
#7132=ORIENTED_EDGE('',*,*,#5166,.F.);
#7133=ORIENTED_EDGE('',*,*,#5208,.T.);
#7134=ORIENTED_EDGE('',*,*,#5205,.T.);
#7135=ORIENTED_EDGE('',*,*,#5162,.F.);
#7136=ORIENTED_EDGE('',*,*,#5213,.T.);
#7137=ORIENTED_EDGE('',*,*,#5210,.T.);
#7138=ORIENTED_EDGE('',*,*,#5158,.F.);
#7139=ORIENTED_EDGE('',*,*,#5218,.T.);
#7140=ORIENTED_EDGE('',*,*,#5215,.T.);
#7141=ORIENTED_EDGE('',*,*,#5154,.F.);
#7142=ORIENTED_EDGE('',*,*,#5223,.T.);
#7143=ORIENTED_EDGE('',*,*,#5220,.T.);
#7144=ORIENTED_EDGE('',*,*,#5150,.F.);
#7145=ORIENTED_EDGE('',*,*,#5228,.T.);
#7146=ORIENTED_EDGE('',*,*,#5225,.T.);
#7147=ORIENTED_EDGE('',*,*,#5146,.F.);
#7148=ORIENTED_EDGE('',*,*,#5233,.T.);
#7149=ORIENTED_EDGE('',*,*,#5230,.T.);
#7150=ORIENTED_EDGE('',*,*,#5142,.F.);
#7151=ORIENTED_EDGE('',*,*,#5238,.T.);
#7152=ORIENTED_EDGE('',*,*,#5235,.T.);
#7153=ORIENTED_EDGE('',*,*,#5138,.F.);
#7154=ORIENTED_EDGE('',*,*,#5243,.T.);
#7155=ORIENTED_EDGE('',*,*,#5240,.T.);
#7156=ORIENTED_EDGE('',*,*,#5134,.F.);
#7157=ORIENTED_EDGE('',*,*,#5248,.T.);
#7158=ORIENTED_EDGE('',*,*,#5245,.T.);
#7159=ORIENTED_EDGE('',*,*,#5130,.F.);
#7160=ORIENTED_EDGE('',*,*,#5253,.T.);
#7161=ORIENTED_EDGE('',*,*,#5250,.T.);
#7162=ORIENTED_EDGE('',*,*,#5126,.F.);
#7163=ORIENTED_EDGE('',*,*,#5258,.T.);
#7164=ORIENTED_EDGE('',*,*,#5255,.T.);
#7165=ORIENTED_EDGE('',*,*,#5122,.F.);
#7166=ORIENTED_EDGE('',*,*,#5263,.T.);
#7167=ORIENTED_EDGE('',*,*,#5260,.T.);
#7168=ORIENTED_EDGE('',*,*,#5118,.F.);
#7169=ORIENTED_EDGE('',*,*,#5268,.T.);
#7170=ORIENTED_EDGE('',*,*,#5265,.T.);
#7171=ORIENTED_EDGE('',*,*,#5114,.F.);
#7172=ORIENTED_EDGE('',*,*,#5273,.T.);
#7173=ORIENTED_EDGE('',*,*,#5270,.T.);
#7174=ORIENTED_EDGE('',*,*,#5110,.F.);
#7175=ORIENTED_EDGE('',*,*,#5278,.T.);
#7176=ORIENTED_EDGE('',*,*,#5275,.T.);
#7177=ORIENTED_EDGE('',*,*,#5106,.F.);
#7178=ORIENTED_EDGE('',*,*,#5283,.T.);
#7179=ORIENTED_EDGE('',*,*,#5280,.T.);
#7180=ORIENTED_EDGE('',*,*,#5102,.F.);
#7181=ORIENTED_EDGE('',*,*,#5288,.T.);
#7182=ORIENTED_EDGE('',*,*,#5285,.T.);
#7183=ORIENTED_EDGE('',*,*,#5098,.F.);
#7184=ORIENTED_EDGE('',*,*,#5293,.T.);
#7185=ORIENTED_EDGE('',*,*,#5290,.T.);
#7186=ORIENTED_EDGE('',*,*,#5094,.F.);
#7187=ORIENTED_EDGE('',*,*,#5298,.T.);
#7188=ORIENTED_EDGE('',*,*,#5295,.T.);
#7189=ORIENTED_EDGE('',*,*,#5090,.F.);
#7190=ORIENTED_EDGE('',*,*,#5303,.T.);
#7191=ORIENTED_EDGE('',*,*,#5300,.T.);
#7192=ORIENTED_EDGE('',*,*,#5086,.F.);
#7193=ORIENTED_EDGE('',*,*,#5308,.T.);
#7194=ORIENTED_EDGE('',*,*,#5305,.T.);
#7195=ORIENTED_EDGE('',*,*,#5082,.F.);
#7196=ORIENTED_EDGE('',*,*,#5313,.T.);
#7197=ORIENTED_EDGE('',*,*,#5310,.T.);
#7198=ORIENTED_EDGE('',*,*,#5078,.F.);
#7199=ORIENTED_EDGE('',*,*,#5397,.F.);
#7200=ORIENTED_EDGE('',*,*,#5420,.F.);
#7201=ORIENTED_EDGE('',*,*,#5423,.F.);
#7202=ORIENTED_EDGE('',*,*,#5423,.T.);
#7203=ORIENTED_EDGE('',*,*,#5418,.F.);
#7204=ORIENTED_EDGE('',*,*,#5424,.F.);
#7205=ORIENTED_EDGE('',*,*,#5398,.F.);
#7206=ORIENTED_EDGE('',*,*,#5424,.T.);
#7207=ORIENTED_EDGE('',*,*,#5386,.F.);
#7208=ORIENTED_EDGE('',*,*,#5425,.F.);
#7209=ORIENTED_EDGE('',*,*,#5394,.F.);
#7210=ORIENTED_EDGE('',*,*,#5425,.T.);
#7211=ORIENTED_EDGE('',*,*,#5412,.F.);
#7212=ORIENTED_EDGE('',*,*,#5426,.F.);
#7213=ORIENTED_EDGE('',*,*,#5395,.F.);
#7214=ORIENTED_EDGE('',*,*,#5414,.F.);
#7215=ORIENTED_EDGE('',*,*,#5396,.F.);
#7216=ORIENTED_EDGE('',*,*,#5426,.T.);
#7217=ORIENTED_EDGE('',*,*,#5415,.F.);
#7218=ORIENTED_EDGE('',*,*,#5390,.F.);
#7219=ORIENTED_EDGE('',*,*,#5427,.F.);
#7220=ORIENTED_EDGE('',*,*,#5427,.T.);
#7221=ORIENTED_EDGE('',*,*,#5389,.F.);
#7222=ORIENTED_EDGE('',*,*,#5428,.F.);
#7223=ORIENTED_EDGE('',*,*,#5417,.F.);
#7224=ORIENTED_EDGE('',*,*,#5428,.T.);
#7225=ORIENTED_EDGE('',*,*,#5393,.F.);
#7226=ORIENTED_EDGE('',*,*,#5429,.F.);
#7227=ORIENTED_EDGE('',*,*,#5388,.F.);
#7228=ORIENTED_EDGE('',*,*,#5429,.T.);
#7229=ORIENTED_EDGE('',*,*,#5392,.F.);
#7230=ORIENTED_EDGE('',*,*,#5430,.F.);
#7231=ORIENTED_EDGE('',*,*,#5413,.F.);
#7232=ORIENTED_EDGE('',*,*,#5391,.F.);
#7233=ORIENTED_EDGE('',*,*,#5410,.F.);
#7234=ORIENTED_EDGE('',*,*,#5430,.T.);
#7235=ORIENTED_EDGE('',*,*,#5400,.F.);
#7236=ORIENTED_EDGE('',*,*,#5431,.T.);
#7237=ORIENTED_EDGE('',*,*,#5432,.T.);
#7238=ORIENTED_EDGE('',*,*,#5433,.T.);
#7239=ORIENTED_EDGE('',*,*,#5434,.T.);
#7240=ORIENTED_EDGE('',*,*,#5433,.F.);
#7241=ORIENTED_EDGE('',*,*,#5434,.F.);
#7242=ORIENTED_EDGE('',*,*,#5435,.T.);
#7243=ORIENTED_EDGE('',*,*,#5436,.T.);
#7244=ORIENTED_EDGE('',*,*,#5435,.F.);
#7245=ORIENTED_EDGE('',*,*,#5437,.F.);
#7246=ORIENTED_EDGE('',*,*,#5438,.F.);
#7247=ORIENTED_EDGE('',*,*,#5439,.F.);
#7248=ORIENTED_EDGE('',*,*,#5440,.F.);
#7249=ORIENTED_EDGE('',*,*,#5436,.F.);
#7250=ORIENTED_EDGE('',*,*,#5441,.T.);
#7251=ORIENTED_EDGE('',*,*,#5442,.T.);
#7252=ORIENTED_EDGE('',*,*,#5441,.F.);
#7253=ORIENTED_EDGE('',*,*,#5431,.F.);
#7254=ORIENTED_EDGE('',*,*,#5443,.T.);
#7255=ORIENTED_EDGE('',*,*,#5432,.F.);
#7256=ORIENTED_EDGE('',*,*,#5443,.F.);
#7257=ORIENTED_EDGE('',*,*,#5437,.T.);
#7258=ORIENTED_EDGE('',*,*,#5444,.T.);
#7259=ORIENTED_EDGE('',*,*,#5440,.T.);
#7260=ORIENTED_EDGE('',*,*,#5439,.T.);
#7261=ORIENTED_EDGE('',*,*,#5444,.F.);
#7262=ORIENTED_EDGE('',*,*,#5438,.T.);
#7263=ORIENTED_EDGE('',*,*,#5442,.F.);
#7264=ORIENTED_EDGE('',*,*,#5445,.F.);
#7265=ORIENTED_EDGE('',*,*,#5446,.F.);
#7266=ORIENTED_EDGE('',*,*,#5447,.F.);
#7267=ORIENTED_EDGE('',*,*,#5448,.F.);
#7268=ORIENTED_EDGE('',*,*,#5446,.T.);
#7269=ORIENTED_EDGE('',*,*,#5449,.F.);
#7270=ORIENTED_EDGE('',*,*,#5450,.F.);
#7271=ORIENTED_EDGE('',*,*,#5451,.T.);
#7272=ORIENTED_EDGE('',*,*,#5447,.T.);
#7273=ORIENTED_EDGE('',*,*,#5451,.F.);
#7274=ORIENTED_EDGE('',*,*,#5452,.F.);
#7275=ORIENTED_EDGE('',*,*,#5453,.T.);
#7276=ORIENTED_EDGE('',*,*,#5448,.T.);
#7277=ORIENTED_EDGE('',*,*,#5453,.F.);
#7278=ORIENTED_EDGE('',*,*,#5454,.F.);
#7279=ORIENTED_EDGE('',*,*,#5455,.T.);
#7280=ORIENTED_EDGE('',*,*,#5445,.T.);
#7281=ORIENTED_EDGE('',*,*,#5455,.F.);
#7282=ORIENTED_EDGE('',*,*,#5456,.F.);
#7283=ORIENTED_EDGE('',*,*,#5449,.T.);
#7284=ORIENTED_EDGE('',*,*,#5450,.T.);
#7285=ORIENTED_EDGE('',*,*,#5456,.T.);
#7286=ORIENTED_EDGE('',*,*,#5454,.T.);
#7287=ORIENTED_EDGE('',*,*,#5452,.T.);
#7288=ORIENTED_EDGE('',*,*,#5457,.F.);
#7289=ORIENTED_EDGE('',*,*,#5458,.T.);
#7290=ORIENTED_EDGE('',*,*,#5459,.T.);
#7291=ORIENTED_EDGE('',*,*,#5460,.F.);
#7292=ORIENTED_EDGE('',*,*,#5461,.F.);
#7293=ORIENTED_EDGE('',*,*,#5460,.T.);
#7294=ORIENTED_EDGE('',*,*,#5462,.T.);
#7295=ORIENTED_EDGE('',*,*,#5463,.F.);
#7296=ORIENTED_EDGE('',*,*,#5464,.F.);
#7297=ORIENTED_EDGE('',*,*,#5463,.T.);
#7298=ORIENTED_EDGE('',*,*,#5465,.T.);
#7299=ORIENTED_EDGE('',*,*,#5466,.F.);
#7300=ORIENTED_EDGE('',*,*,#5467,.F.);
#7301=ORIENTED_EDGE('',*,*,#5466,.T.);
#7302=ORIENTED_EDGE('',*,*,#5468,.T.);
#7303=ORIENTED_EDGE('',*,*,#5469,.F.);
#7304=ORIENTED_EDGE('',*,*,#5470,.F.);
#7305=ORIENTED_EDGE('',*,*,#5469,.T.);
#7306=ORIENTED_EDGE('',*,*,#5471,.T.);
#7307=ORIENTED_EDGE('',*,*,#5472,.F.);
#7308=ORIENTED_EDGE('',*,*,#5473,.F.);
#7309=ORIENTED_EDGE('',*,*,#5474,.F.);
#7310=ORIENTED_EDGE('',*,*,#5472,.T.);
#7311=ORIENTED_EDGE('',*,*,#5475,.T.);
#7312=ORIENTED_EDGE('',*,*,#5476,.F.);
#7313=ORIENTED_EDGE('',*,*,#5477,.F.);
#7314=ORIENTED_EDGE('',*,*,#5476,.T.);
#7315=ORIENTED_EDGE('',*,*,#5478,.T.);
#7316=ORIENTED_EDGE('',*,*,#5479,.F.);
#7317=ORIENTED_EDGE('',*,*,#5480,.F.);
#7318=ORIENTED_EDGE('',*,*,#5481,.F.);
#7319=ORIENTED_EDGE('',*,*,#5479,.T.);
#7320=ORIENTED_EDGE('',*,*,#5482,.T.);
#7321=ORIENTED_EDGE('',*,*,#5458,.F.);
#7322=ORIENTED_EDGE('',*,*,#5483,.T.);
#7323=ORIENTED_EDGE('',*,*,#5484,.T.);
#7324=ORIENTED_EDGE('',*,*,#5485,.F.);
#7325=ORIENTED_EDGE('',*,*,#5486,.T.);
#7326=ORIENTED_EDGE('',*,*,#5487,.T.);
#7327=ORIENTED_EDGE('',*,*,#5486,.F.);
#7328=ORIENTED_EDGE('',*,*,#5488,.F.);
#7329=ORIENTED_EDGE('',*,*,#5489,.F.);
#7330=ORIENTED_EDGE('',*,*,#5490,.F.);
#7331=ORIENTED_EDGE('',*,*,#5484,.F.);
#7332=ORIENTED_EDGE('',*,*,#5491,.F.);
#7333=ORIENTED_EDGE('',*,*,#5492,.F.);
#7334=ORIENTED_EDGE('',*,*,#5493,.T.);
#7335=ORIENTED_EDGE('',*,*,#5494,.T.);
#7336=ORIENTED_EDGE('',*,*,#5491,.T.);
#7337=ORIENTED_EDGE('',*,*,#5494,.F.);
#7338=ORIENTED_EDGE('',*,*,#5495,.T.);
#7339=ORIENTED_EDGE('',*,*,#5496,.T.);
#7340=ORIENTED_EDGE('',*,*,#5487,.F.);
#7341=ORIENTED_EDGE('',*,*,#5497,.F.);
#7342=ORIENTED_EDGE('',*,*,#5498,.T.);
#7343=ORIENTED_EDGE('',*,*,#5492,.T.);
#7344=ORIENTED_EDGE('',*,*,#5498,.F.);
#7345=ORIENTED_EDGE('',*,*,#5497,.T.);
#7346=ORIENTED_EDGE('',*,*,#5499,.T.);
#7347=ORIENTED_EDGE('',*,*,#5500,.F.);
#7348=ORIENTED_EDGE('',*,*,#5501,.T.);
#7349=ORIENTED_EDGE('',*,*,#5502,.F.);
#7350=ORIENTED_EDGE('',*,*,#5503,.F.);
#7351=ORIENTED_EDGE('',*,*,#5504,.T.);
#7352=ORIENTED_EDGE('',*,*,#5502,.T.);
#7353=ORIENTED_EDGE('',*,*,#5504,.F.);
#7354=ORIENTED_EDGE('',*,*,#5483,.F.);
#7355=ORIENTED_EDGE('',*,*,#5503,.T.);
#7356=ORIENTED_EDGE('',*,*,#5505,.T.);
#7357=ORIENTED_EDGE('',*,*,#5459,.F.);
#7358=ORIENTED_EDGE('',*,*,#5482,.F.);
#7359=ORIENTED_EDGE('',*,*,#5478,.F.);
#7360=ORIENTED_EDGE('',*,*,#5475,.F.);
#7361=ORIENTED_EDGE('',*,*,#5471,.F.);
#7362=ORIENTED_EDGE('',*,*,#5468,.F.);
#7363=ORIENTED_EDGE('',*,*,#5465,.F.);
#7364=ORIENTED_EDGE('',*,*,#5462,.F.);
#7365=ORIENTED_EDGE('',*,*,#5505,.F.);
#7366=ORIENTED_EDGE('',*,*,#5506,.T.);
#7367=ORIENTED_EDGE('',*,*,#5501,.F.);
#7368=ORIENTED_EDGE('',*,*,#5506,.F.);
#7369=ORIENTED_EDGE('',*,*,#5507,.T.);
#7370=ORIENTED_EDGE('',*,*,#5508,.T.);
#7371=ORIENTED_EDGE('',*,*,#5500,.T.);
#7372=ORIENTED_EDGE('',*,*,#5508,.F.);
#7373=ORIENTED_EDGE('',*,*,#5509,.F.);
#7374=ORIENTED_EDGE('',*,*,#5510,.T.);
#7375=ORIENTED_EDGE('',*,*,#5511,.T.);
#7376=ORIENTED_EDGE('',*,*,#5512,.T.);
#7377=ORIENTED_EDGE('',*,*,#5513,.T.);
#7378=ORIENTED_EDGE('',*,*,#5512,.F.);
#7379=ORIENTED_EDGE('',*,*,#5514,.T.);
#7380=ORIENTED_EDGE('',*,*,#5515,.T.);
#7381=ORIENTED_EDGE('',*,*,#5516,.T.);
#7382=ORIENTED_EDGE('',*,*,#5510,.F.);
#7383=ORIENTED_EDGE('',*,*,#5509,.T.);
#7384=ORIENTED_EDGE('',*,*,#5490,.T.);
#7385=ORIENTED_EDGE('',*,*,#5517,.T.);
#7386=ORIENTED_EDGE('',*,*,#5516,.F.);
#7387=ORIENTED_EDGE('',*,*,#5518,.T.);
#7388=ORIENTED_EDGE('',*,*,#5519,.F.);
#7389=ORIENTED_EDGE('',*,*,#5485,.T.);
#7390=ORIENTED_EDGE('',*,*,#5518,.F.);
#7391=ORIENTED_EDGE('',*,*,#5515,.F.);
#7392=ORIENTED_EDGE('',*,*,#5520,.T.);
#7393=ORIENTED_EDGE('',*,*,#5489,.T.);
#7394=ORIENTED_EDGE('',*,*,#5521,.T.);
#7395=ORIENTED_EDGE('',*,*,#5511,.F.);
#7396=ORIENTED_EDGE('',*,*,#5517,.F.);
#7397=ORIENTED_EDGE('',*,*,#5488,.T.);
#7398=ORIENTED_EDGE('',*,*,#5520,.F.);
#7399=ORIENTED_EDGE('',*,*,#5514,.F.);
#7400=ORIENTED_EDGE('',*,*,#5521,.F.);
#7401=ORIENTED_EDGE('',*,*,#5507,.F.);
#7402=ORIENTED_EDGE('',*,*,#5522,.T.);
#7403=ORIENTED_EDGE('',*,*,#5522,.F.);
#7404=ORIENTED_EDGE('',*,*,#5523,.T.);
#7405=ORIENTED_EDGE('',*,*,#5519,.T.);
#7406=ORIENTED_EDGE('',*,*,#5523,.F.);
#7407=ORIENTED_EDGE('',*,*,#5524,.F.);
#7408=ORIENTED_EDGE('',*,*,#5525,.T.);
#7409=ORIENTED_EDGE('',*,*,#5480,.T.);
#7410=ORIENTED_EDGE('',*,*,#5525,.F.);
#7411=ORIENTED_EDGE('',*,*,#5524,.T.);
#7412=ORIENTED_EDGE('',*,*,#5457,.T.);
#7413=ORIENTED_EDGE('',*,*,#5461,.T.);
#7414=ORIENTED_EDGE('',*,*,#5464,.T.);
#7415=ORIENTED_EDGE('',*,*,#5467,.T.);
#7416=ORIENTED_EDGE('',*,*,#5470,.T.);
#7417=ORIENTED_EDGE('',*,*,#5526,.T.);
#7418=ORIENTED_EDGE('',*,*,#5527,.F.);
#7419=ORIENTED_EDGE('',*,*,#5526,.F.);
#7420=ORIENTED_EDGE('',*,*,#5473,.T.);
#7421=ORIENTED_EDGE('',*,*,#5474,.T.);
#7422=ORIENTED_EDGE('',*,*,#5477,.T.);
#7423=ORIENTED_EDGE('',*,*,#5481,.T.);
#7424=ORIENTED_EDGE('',*,*,#5527,.T.);
#7425=ORIENTED_EDGE('',*,*,#5493,.F.);
#7426=ORIENTED_EDGE('',*,*,#5528,.T.);
#7427=ORIENTED_EDGE('',*,*,#5496,.F.);
#7428=ORIENTED_EDGE('',*,*,#5528,.F.);
#7429=ORIENTED_EDGE('',*,*,#5495,.F.);
#7430=ORIENTED_EDGE('',*,*,#5513,.F.);
#7431=ORIENTED_EDGE('',*,*,#5529,.T.);
#7432=ORIENTED_EDGE('',*,*,#5499,.F.);
#7433=ORIENTED_EDGE('',*,*,#5529,.F.);
#7434=ORIENTED_EDGE('',*,*,#5530,.T.);
#7435=ORIENTED_EDGE('',*,*,#5531,.T.);
#7436=ORIENTED_EDGE('',*,*,#5532,.F.);
#7437=ORIENTED_EDGE('',*,*,#5533,.F.);
#7438=ORIENTED_EDGE('',*,*,#5534,.F.);
#7439=ORIENTED_EDGE('',*,*,#5535,.F.);
#7440=ORIENTED_EDGE('',*,*,#5536,.T.);
#7441=ORIENTED_EDGE('',*,*,#5537,.T.);
#7442=ORIENTED_EDGE('',*,*,#5538,.T.);
#7443=ORIENTED_EDGE('',*,*,#5539,.F.);
#7444=ORIENTED_EDGE('',*,*,#5540,.F.);
#7445=ORIENTED_EDGE('',*,*,#5535,.T.);
#7446=ORIENTED_EDGE('',*,*,#5541,.T.);
#7447=ORIENTED_EDGE('',*,*,#5537,.F.);
#7448=ORIENTED_EDGE('',*,*,#5542,.F.);
#7449=ORIENTED_EDGE('',*,*,#5543,.T.);
#7450=ORIENTED_EDGE('',*,*,#5536,.F.);
#7451=ORIENTED_EDGE('',*,*,#5540,.T.);
#7452=ORIENTED_EDGE('',*,*,#5544,.T.);
#7453=ORIENTED_EDGE('',*,*,#5545,.T.);
#7454=ORIENTED_EDGE('',*,*,#5546,.T.);
#7455=ORIENTED_EDGE('',*,*,#5547,.T.);
#7456=ORIENTED_EDGE('',*,*,#5548,.T.);
#7457=ORIENTED_EDGE('',*,*,#5549,.T.);
#7458=ORIENTED_EDGE('',*,*,#5550,.T.);
#7459=ORIENTED_EDGE('',*,*,#5551,.T.);
#7460=ORIENTED_EDGE('',*,*,#5533,.T.);
#7461=ORIENTED_EDGE('',*,*,#5552,.F.);
#7462=ORIENTED_EDGE('',*,*,#5553,.F.);
#7463=ORIENTED_EDGE('',*,*,#5554,.F.);
#7464=ORIENTED_EDGE('',*,*,#5555,.F.);
#7465=ORIENTED_EDGE('',*,*,#5556,.F.);
#7466=ORIENTED_EDGE('',*,*,#5557,.F.);
#7467=ORIENTED_EDGE('',*,*,#5558,.F.);
#7468=ORIENTED_EDGE('',*,*,#5559,.F.);
#7469=ORIENTED_EDGE('',*,*,#5542,.T.);
#7470=ORIENTED_EDGE('',*,*,#5560,.T.);
#7471=ORIENTED_EDGE('',*,*,#5534,.T.);
#7472=ORIENTED_EDGE('',*,*,#5541,.F.);
#7473=ORIENTED_EDGE('',*,*,#5561,.T.);
#7474=ORIENTED_EDGE('',*,*,#5562,.T.);
#7475=ORIENTED_EDGE('',*,*,#5563,.T.);
#7476=ORIENTED_EDGE('',*,*,#5564,.T.);
#7477=ORIENTED_EDGE('',*,*,#5565,.T.);
#7478=ORIENTED_EDGE('',*,*,#5566,.T.);
#7479=ORIENTED_EDGE('',*,*,#5567,.T.);
#7480=ORIENTED_EDGE('',*,*,#5568,.T.);
#7481=ORIENTED_EDGE('',*,*,#5531,.F.);
#7482=ORIENTED_EDGE('',*,*,#5569,.F.);
#7483=ORIENTED_EDGE('',*,*,#5570,.F.);
#7484=ORIENTED_EDGE('',*,*,#5571,.F.);
#7485=ORIENTED_EDGE('',*,*,#5572,.F.);
#7486=ORIENTED_EDGE('',*,*,#5573,.F.);
#7487=ORIENTED_EDGE('',*,*,#5574,.F.);
#7488=ORIENTED_EDGE('',*,*,#5575,.F.);
#7489=ORIENTED_EDGE('',*,*,#5576,.F.);
#7490=ORIENTED_EDGE('',*,*,#5538,.F.);
#7491=ORIENTED_EDGE('',*,*,#5577,.T.);
#7492=ORIENTED_EDGE('',*,*,#5578,.T.);
#7493=ORIENTED_EDGE('',*,*,#5579,.T.);
#7494=ORIENTED_EDGE('',*,*,#5580,.T.);
#7495=ORIENTED_EDGE('',*,*,#5579,.F.);
#7496=ORIENTED_EDGE('',*,*,#5581,.T.);
#7497=ORIENTED_EDGE('',*,*,#5561,.F.);
#7498=ORIENTED_EDGE('',*,*,#5543,.F.);
#7499=ORIENTED_EDGE('',*,*,#5559,.T.);
#7500=ORIENTED_EDGE('',*,*,#5582,.T.);
#7501=ORIENTED_EDGE('',*,*,#5562,.F.);
#7502=ORIENTED_EDGE('',*,*,#5582,.F.);
#7503=ORIENTED_EDGE('',*,*,#5558,.T.);
#7504=ORIENTED_EDGE('',*,*,#5583,.T.);
#7505=ORIENTED_EDGE('',*,*,#5563,.F.);
#7506=ORIENTED_EDGE('',*,*,#5583,.F.);
#7507=ORIENTED_EDGE('',*,*,#5557,.T.);
#7508=ORIENTED_EDGE('',*,*,#5584,.T.);
#7509=ORIENTED_EDGE('',*,*,#5564,.F.);
#7510=ORIENTED_EDGE('',*,*,#5584,.F.);
#7511=ORIENTED_EDGE('',*,*,#5556,.T.);
#7512=ORIENTED_EDGE('',*,*,#5585,.T.);
#7513=ORIENTED_EDGE('',*,*,#5565,.F.);
#7514=ORIENTED_EDGE('',*,*,#5585,.F.);
#7515=ORIENTED_EDGE('',*,*,#5555,.T.);
#7516=ORIENTED_EDGE('',*,*,#5586,.T.);
#7517=ORIENTED_EDGE('',*,*,#5566,.F.);
#7518=ORIENTED_EDGE('',*,*,#5586,.F.);
#7519=ORIENTED_EDGE('',*,*,#5554,.T.);
#7520=ORIENTED_EDGE('',*,*,#5587,.T.);
#7521=ORIENTED_EDGE('',*,*,#5567,.F.);
#7522=ORIENTED_EDGE('',*,*,#5587,.F.);
#7523=ORIENTED_EDGE('',*,*,#5553,.T.);
#7524=ORIENTED_EDGE('',*,*,#5588,.T.);
#7525=ORIENTED_EDGE('',*,*,#5568,.F.);
#7526=ORIENTED_EDGE('',*,*,#5588,.F.);
#7527=ORIENTED_EDGE('',*,*,#5552,.T.);
#7528=ORIENTED_EDGE('',*,*,#5532,.T.);
#7529=ORIENTED_EDGE('',*,*,#5576,.T.);
#7530=ORIENTED_EDGE('',*,*,#5589,.F.);
#7531=ORIENTED_EDGE('',*,*,#5544,.F.);
#7532=ORIENTED_EDGE('',*,*,#5539,.T.);
#7533=ORIENTED_EDGE('',*,*,#5575,.T.);
#7534=ORIENTED_EDGE('',*,*,#5590,.F.);
#7535=ORIENTED_EDGE('',*,*,#5545,.F.);
#7536=ORIENTED_EDGE('',*,*,#5589,.T.);
#7537=ORIENTED_EDGE('',*,*,#5574,.T.);
#7538=ORIENTED_EDGE('',*,*,#5591,.F.);
#7539=ORIENTED_EDGE('',*,*,#5546,.F.);
#7540=ORIENTED_EDGE('',*,*,#5590,.T.);
#7541=ORIENTED_EDGE('',*,*,#5573,.T.);
#7542=ORIENTED_EDGE('',*,*,#5592,.F.);
#7543=ORIENTED_EDGE('',*,*,#5547,.F.);
#7544=ORIENTED_EDGE('',*,*,#5591,.T.);
#7545=ORIENTED_EDGE('',*,*,#5572,.T.);
#7546=ORIENTED_EDGE('',*,*,#5593,.F.);
#7547=ORIENTED_EDGE('',*,*,#5548,.F.);
#7548=ORIENTED_EDGE('',*,*,#5592,.T.);
#7549=ORIENTED_EDGE('',*,*,#5571,.T.);
#7550=ORIENTED_EDGE('',*,*,#5594,.F.);
#7551=ORIENTED_EDGE('',*,*,#5549,.F.);
#7552=ORIENTED_EDGE('',*,*,#5593,.T.);
#7553=ORIENTED_EDGE('',*,*,#5570,.T.);
#7554=ORIENTED_EDGE('',*,*,#5595,.F.);
#7555=ORIENTED_EDGE('',*,*,#5550,.F.);
#7556=ORIENTED_EDGE('',*,*,#5594,.T.);
#7557=ORIENTED_EDGE('',*,*,#5569,.T.);
#7558=ORIENTED_EDGE('',*,*,#5530,.F.);
#7559=ORIENTED_EDGE('',*,*,#5551,.F.);
#7560=ORIENTED_EDGE('',*,*,#5595,.T.);
#7561=ORIENTED_EDGE('',*,*,#5578,.F.);
#7562=ORIENTED_EDGE('',*,*,#5596,.T.);
#7563=ORIENTED_EDGE('',*,*,#5577,.F.);
#7564=ORIENTED_EDGE('',*,*,#5596,.F.);
#7565=ORIENTED_EDGE('',*,*,#5581,.F.);
#7566=ORIENTED_EDGE('',*,*,#5580,.F.);
#7567=ORIENTED_EDGE('',*,*,#5597,.T.);
#7568=ORIENTED_EDGE('',*,*,#5560,.F.);
#7569=ORIENTED_EDGE('',*,*,#5597,.F.);
#7570=ORIENTED_EDGE('',*,*,#5598,.T.);
#7571=ORIENTED_EDGE('',*,*,#5599,.T.);
#7572=ORIENTED_EDGE('',*,*,#5600,.T.);
#7573=ORIENTED_EDGE('',*,*,#5601,.T.);
#7574=ORIENTED_EDGE('',*,*,#5600,.F.);
#7575=ORIENTED_EDGE('',*,*,#5602,.T.);
#7576=ORIENTED_EDGE('',*,*,#5603,.T.);
#7577=ORIENTED_EDGE('',*,*,#5598,.F.);
#7578=ORIENTED_EDGE('',*,*,#5599,.F.);
#7579=ORIENTED_EDGE('',*,*,#5604,.T.);
#7580=ORIENTED_EDGE('',*,*,#5603,.F.);
#7581=ORIENTED_EDGE('',*,*,#5604,.F.);
#7582=ORIENTED_EDGE('',*,*,#5601,.F.);
#7583=ORIENTED_EDGE('',*,*,#5605,.T.);
#7584=ORIENTED_EDGE('',*,*,#5602,.F.);
#7585=ORIENTED_EDGE('',*,*,#5605,.F.);
#7586=ORIENTED_EDGE('',*,*,#5606,.T.);
#7587=ORIENTED_EDGE('',*,*,#5607,.T.);
#7588=ORIENTED_EDGE('',*,*,#5608,.T.);
#7589=ORIENTED_EDGE('',*,*,#5609,.T.);
#7590=ORIENTED_EDGE('',*,*,#5608,.F.);
#7591=ORIENTED_EDGE('',*,*,#5610,.T.);
#7592=ORIENTED_EDGE('',*,*,#5611,.F.);
#7593=ORIENTED_EDGE('',*,*,#5612,.F.);
#7594=ORIENTED_EDGE('',*,*,#5613,.T.);
#7595=ORIENTED_EDGE('',*,*,#5609,.F.);
#7596=ORIENTED_EDGE('',*,*,#5614,.T.);
#7597=ORIENTED_EDGE('',*,*,#5615,.T.);
#7598=ORIENTED_EDGE('',*,*,#5616,.T.);
#7599=ORIENTED_EDGE('',*,*,#5615,.F.);
#7600=ORIENTED_EDGE('',*,*,#5617,.T.);
#7601=ORIENTED_EDGE('',*,*,#5616,.F.);
#7602=ORIENTED_EDGE('',*,*,#5618,.F.);
#7603=ORIENTED_EDGE('',*,*,#5619,.T.);
#7604=ORIENTED_EDGE('',*,*,#5620,.F.);
#7605=ORIENTED_EDGE('',*,*,#5621,.T.);
#7606=ORIENTED_EDGE('',*,*,#5622,.F.);
#7607=ORIENTED_EDGE('',*,*,#5623,.T.);
#7608=ORIENTED_EDGE('',*,*,#5624,.F.);
#7609=ORIENTED_EDGE('',*,*,#5625,.T.);
#7610=ORIENTED_EDGE('',*,*,#5626,.F.);
#7611=ORIENTED_EDGE('',*,*,#5627,.T.);
#7612=ORIENTED_EDGE('',*,*,#5618,.T.);
#7613=ORIENTED_EDGE('',*,*,#5628,.T.);
#7614=ORIENTED_EDGE('',*,*,#5624,.T.);
#7615=ORIENTED_EDGE('',*,*,#5629,.T.);
#7616=ORIENTED_EDGE('',*,*,#5630,.F.);
#7617=ORIENTED_EDGE('',*,*,#5631,.T.);
#7618=ORIENTED_EDGE('',*,*,#5622,.T.);
#7619=ORIENTED_EDGE('',*,*,#5632,.T.);
#7620=ORIENTED_EDGE('',*,*,#5633,.F.);
#7621=ORIENTED_EDGE('',*,*,#5634,.T.);
#7622=ORIENTED_EDGE('',*,*,#5620,.T.);
#7623=ORIENTED_EDGE('',*,*,#5635,.T.);
#7624=ORIENTED_EDGE('',*,*,#5636,.F.);
#7625=ORIENTED_EDGE('',*,*,#5637,.T.);
#7626=ORIENTED_EDGE('',*,*,#5636,.T.);
#7627=ORIENTED_EDGE('',*,*,#5638,.T.);
#7628=ORIENTED_EDGE('',*,*,#5626,.T.);
#7629=ORIENTED_EDGE('',*,*,#5639,.T.);
#7630=ORIENTED_EDGE('',*,*,#5630,.T.);
#7631=ORIENTED_EDGE('',*,*,#5640,.T.);
#7632=ORIENTED_EDGE('',*,*,#5633,.T.);
#7633=ORIENTED_EDGE('',*,*,#5641,.T.);
#7634=ORIENTED_EDGE('',*,*,#5642,.F.);
#7635=ORIENTED_EDGE('',*,*,#5643,.T.);
#7636=ORIENTED_EDGE('',*,*,#5612,.T.);
#7637=ORIENTED_EDGE('',*,*,#5611,.T.);
#7638=ORIENTED_EDGE('',*,*,#5643,.F.);
#7639=ORIENTED_EDGE('',*,*,#5642,.T.);
#7640=ORIENTED_EDGE('',*,*,#5607,.F.);
#7641=ORIENTED_EDGE('',*,*,#5644,.T.);
#7642=ORIENTED_EDGE('',*,*,#5606,.F.);
#7643=ORIENTED_EDGE('',*,*,#5644,.F.);
#7644=ORIENTED_EDGE('',*,*,#5610,.F.);
#7645=ORIENTED_EDGE('',*,*,#5614,.F.);
#7646=ORIENTED_EDGE('',*,*,#5645,.T.);
#7647=ORIENTED_EDGE('',*,*,#5613,.F.);
#7648=ORIENTED_EDGE('',*,*,#5645,.F.);
#7649=ORIENTED_EDGE('',*,*,#5617,.F.);
#7650=ORIENTED_EDGE('',*,*,#5638,.F.);
#7651=ORIENTED_EDGE('',*,*,#5635,.F.);
#7652=ORIENTED_EDGE('',*,*,#5619,.F.);
#7653=ORIENTED_EDGE('',*,*,#5627,.F.);
#7654=ORIENTED_EDGE('',*,*,#5641,.F.);
#7655=ORIENTED_EDGE('',*,*,#5632,.F.);
#7656=ORIENTED_EDGE('',*,*,#5621,.F.);
#7657=ORIENTED_EDGE('',*,*,#5637,.F.);
#7658=ORIENTED_EDGE('',*,*,#5640,.F.);
#7659=ORIENTED_EDGE('',*,*,#5629,.F.);
#7660=ORIENTED_EDGE('',*,*,#5623,.F.);
#7661=ORIENTED_EDGE('',*,*,#5634,.F.);
#7662=ORIENTED_EDGE('',*,*,#5639,.F.);
#7663=ORIENTED_EDGE('',*,*,#5628,.F.);
#7664=ORIENTED_EDGE('',*,*,#5625,.F.);
#7665=ORIENTED_EDGE('',*,*,#5631,.F.);
#7666=ORIENTED_EDGE('',*,*,#5646,.T.);
#7667=ORIENTED_EDGE('',*,*,#5647,.F.);
#7668=ORIENTED_EDGE('',*,*,#5648,.F.);
#7669=ORIENTED_EDGE('',*,*,#5649,.F.);
#7670=ORIENTED_EDGE('',*,*,#5650,.T.);
#7671=ORIENTED_EDGE('',*,*,#5650,.F.);
#7672=ORIENTED_EDGE('',*,*,#5651,.F.);
#7673=ORIENTED_EDGE('',*,*,#5652,.T.);
#7674=ORIENTED_EDGE('',*,*,#5653,.T.);
#7675=ORIENTED_EDGE('',*,*,#5654,.T.);
#7676=ORIENTED_EDGE('',*,*,#5652,.F.);
#7677=ORIENTED_EDGE('',*,*,#5655,.F.);
#7678=ORIENTED_EDGE('',*,*,#5656,.T.);
#7679=ORIENTED_EDGE('',*,*,#5657,.T.);
#7680=ORIENTED_EDGE('',*,*,#5653,.F.);
#7681=ORIENTED_EDGE('',*,*,#5656,.F.);
#7682=ORIENTED_EDGE('',*,*,#5658,.F.);
#7683=ORIENTED_EDGE('',*,*,#5648,.T.);
#7684=ORIENTED_EDGE('',*,*,#5647,.T.);
#7685=ORIENTED_EDGE('',*,*,#5659,.T.);
#7686=ORIENTED_EDGE('',*,*,#5659,.F.);
#7687=ORIENTED_EDGE('',*,*,#5646,.F.);
#7688=ORIENTED_EDGE('',*,*,#5654,.F.);
#7689=ORIENTED_EDGE('',*,*,#5657,.F.);
#7690=ORIENTED_EDGE('',*,*,#5658,.T.);
#7691=ORIENTED_EDGE('',*,*,#5655,.T.);
#7692=ORIENTED_EDGE('',*,*,#5651,.T.);
#7693=ORIENTED_EDGE('',*,*,#5649,.T.);
#7694=ORIENTED_EDGE('',*,*,#5660,.T.);
#7695=ORIENTED_EDGE('',*,*,#5661,.F.);
#7696=ORIENTED_EDGE('',*,*,#5662,.F.);
#7697=ORIENTED_EDGE('',*,*,#5663,.F.);
#7698=ORIENTED_EDGE('',*,*,#5664,.T.);
#7699=ORIENTED_EDGE('',*,*,#5664,.F.);
#7700=ORIENTED_EDGE('',*,*,#5665,.F.);
#7701=ORIENTED_EDGE('',*,*,#5666,.T.);
#7702=ORIENTED_EDGE('',*,*,#5667,.T.);
#7703=ORIENTED_EDGE('',*,*,#5668,.T.);
#7704=ORIENTED_EDGE('',*,*,#5666,.F.);
#7705=ORIENTED_EDGE('',*,*,#5669,.F.);
#7706=ORIENTED_EDGE('',*,*,#5670,.T.);
#7707=ORIENTED_EDGE('',*,*,#5671,.T.);
#7708=ORIENTED_EDGE('',*,*,#5667,.F.);
#7709=ORIENTED_EDGE('',*,*,#5670,.F.);
#7710=ORIENTED_EDGE('',*,*,#5672,.F.);
#7711=ORIENTED_EDGE('',*,*,#5662,.T.);
#7712=ORIENTED_EDGE('',*,*,#5661,.T.);
#7713=ORIENTED_EDGE('',*,*,#5673,.T.);
#7714=ORIENTED_EDGE('',*,*,#5673,.F.);
#7715=ORIENTED_EDGE('',*,*,#5660,.F.);
#7716=ORIENTED_EDGE('',*,*,#5668,.F.);
#7717=ORIENTED_EDGE('',*,*,#5671,.F.);
#7718=ORIENTED_EDGE('',*,*,#5672,.T.);
#7719=ORIENTED_EDGE('',*,*,#5669,.T.);
#7720=ORIENTED_EDGE('',*,*,#5665,.T.);
#7721=ORIENTED_EDGE('',*,*,#5663,.T.);
#7722=ORIENTED_EDGE('',*,*,#5674,.T.);
#7723=ORIENTED_EDGE('',*,*,#5674,.F.);
#7724=ORIENTED_EDGE('',*,*,#5675,.F.);
#7725=ORIENTED_EDGE('',*,*,#5676,.T.);
#7726=ORIENTED_EDGE('',*,*,#5675,.T.);
#7727=ORIENTED_EDGE('',*,*,#5676,.F.);
#7728=ORIENTED_EDGE('',*,*,#5677,.F.);
#7729=ORIENTED_EDGE('',*,*,#5678,.T.);
#7730=ORIENTED_EDGE('',*,*,#5679,.F.);
#7731=ORIENTED_EDGE('',*,*,#5680,.F.);
#7732=ORIENTED_EDGE('',*,*,#5681,.F.);
#7733=ORIENTED_EDGE('',*,*,#5682,.T.);
#7734=ORIENTED_EDGE('',*,*,#5683,.F.);
#7735=ORIENTED_EDGE('',*,*,#5682,.F.);
#7736=ORIENTED_EDGE('',*,*,#5684,.F.);
#7737=ORIENTED_EDGE('',*,*,#5685,.F.);
#7738=ORIENTED_EDGE('',*,*,#5686,.F.);
#7739=ORIENTED_EDGE('',*,*,#5678,.F.);
#7740=ORIENTED_EDGE('',*,*,#5687,.F.);
#7741=ORIENTED_EDGE('',*,*,#5688,.F.);
#7742=ORIENTED_EDGE('',*,*,#5689,.F.);
#7743=ORIENTED_EDGE('',*,*,#5690,.F.);
#7744=ORIENTED_EDGE('',*,*,#5691,.F.);
#7745=ORIENTED_EDGE('',*,*,#5692,.F.);
#7746=ORIENTED_EDGE('',*,*,#5693,.F.);
#7747=ORIENTED_EDGE('',*,*,#5694,.F.);
#7748=ORIENTED_EDGE('',*,*,#5695,.F.);
#7749=ORIENTED_EDGE('',*,*,#5696,.F.);
#7750=ORIENTED_EDGE('',*,*,#5697,.F.);
#7751=ORIENTED_EDGE('',*,*,#5698,.F.);
#7752=ORIENTED_EDGE('',*,*,#5699,.F.);
#7753=ORIENTED_EDGE('',*,*,#5700,.F.);
#7754=ORIENTED_EDGE('',*,*,#5701,.F.);
#7755=ORIENTED_EDGE('',*,*,#5702,.F.);
#7756=ORIENTED_EDGE('',*,*,#5703,.F.);
#7757=ORIENTED_EDGE('',*,*,#5704,.F.);
#7758=ORIENTED_EDGE('',*,*,#5705,.F.);
#7759=ORIENTED_EDGE('',*,*,#5706,.F.);
#7760=ORIENTED_EDGE('',*,*,#5707,.F.);
#7761=ORIENTED_EDGE('',*,*,#5708,.F.);
#7762=ORIENTED_EDGE('',*,*,#5709,.F.);
#7763=ORIENTED_EDGE('',*,*,#5710,.F.);
#7764=ORIENTED_EDGE('',*,*,#5711,.F.);
#7765=ORIENTED_EDGE('',*,*,#5712,.F.);
#7766=ORIENTED_EDGE('',*,*,#5713,.F.);
#7767=ORIENTED_EDGE('',*,*,#5714,.F.);
#7768=ORIENTED_EDGE('',*,*,#5715,.F.);
#7769=ORIENTED_EDGE('',*,*,#5716,.F.);
#7770=ORIENTED_EDGE('',*,*,#5717,.F.);
#7771=ORIENTED_EDGE('',*,*,#5718,.F.);
#7772=ORIENTED_EDGE('',*,*,#5719,.F.);
#7773=ORIENTED_EDGE('',*,*,#5720,.F.);
#7774=ORIENTED_EDGE('',*,*,#5721,.F.);
#7775=ORIENTED_EDGE('',*,*,#5722,.F.);
#7776=ORIENTED_EDGE('',*,*,#5723,.F.);
#7777=ORIENTED_EDGE('',*,*,#5724,.T.);
#7778=ORIENTED_EDGE('',*,*,#5725,.T.);
#7779=ORIENTED_EDGE('',*,*,#5726,.T.);
#7780=ORIENTED_EDGE('',*,*,#5727,.T.);
#7781=ORIENTED_EDGE('',*,*,#5728,.T.);
#7782=ORIENTED_EDGE('',*,*,#5727,.F.);
#7783=ORIENTED_EDGE('',*,*,#5729,.T.);
#7784=ORIENTED_EDGE('',*,*,#5730,.T.);
#7785=ORIENTED_EDGE('',*,*,#5724,.F.);
#7786=ORIENTED_EDGE('',*,*,#5731,.T.);
#7787=ORIENTED_EDGE('',*,*,#5732,.T.);
#7788=ORIENTED_EDGE('',*,*,#5733,.T.);
#7789=ORIENTED_EDGE('',*,*,#5734,.T.);
#7790=ORIENTED_EDGE('',*,*,#5735,.T.);
#7791=ORIENTED_EDGE('',*,*,#5736,.T.);
#7792=ORIENTED_EDGE('',*,*,#5737,.T.);
#7793=ORIENTED_EDGE('',*,*,#5738,.F.);
#7794=ORIENTED_EDGE('',*,*,#5737,.F.);
#7795=ORIENTED_EDGE('',*,*,#5739,.T.);
#7796=ORIENTED_EDGE('',*,*,#5740,.T.);
#7797=ORIENTED_EDGE('',*,*,#5735,.F.);
#7798=ORIENTED_EDGE('',*,*,#5741,.T.);
#7799=ORIENTED_EDGE('',*,*,#5742,.T.);
#7800=ORIENTED_EDGE('',*,*,#5743,.T.);
#7801=ORIENTED_EDGE('',*,*,#5744,.T.);
#7802=ORIENTED_EDGE('',*,*,#5745,.T.);
#7803=ORIENTED_EDGE('',*,*,#5746,.T.);
#7804=ORIENTED_EDGE('',*,*,#5747,.T.);
#7805=ORIENTED_EDGE('',*,*,#5748,.T.);
#7806=ORIENTED_EDGE('',*,*,#5749,.T.);
#7807=ORIENTED_EDGE('',*,*,#5750,.T.);
#7808=ORIENTED_EDGE('',*,*,#5751,.T.);
#7809=ORIENTED_EDGE('',*,*,#5752,.T.);
#7810=ORIENTED_EDGE('',*,*,#5753,.T.);
#7811=ORIENTED_EDGE('',*,*,#5754,.T.);
#7812=ORIENTED_EDGE('',*,*,#5753,.F.);
#7813=ORIENTED_EDGE('',*,*,#5755,.T.);
#7814=ORIENTED_EDGE('',*,*,#5756,.T.);
#7815=ORIENTED_EDGE('',*,*,#5750,.F.);
#7816=ORIENTED_EDGE('',*,*,#5757,.T.);
#7817=ORIENTED_EDGE('',*,*,#5758,.T.);
#7818=ORIENTED_EDGE('',*,*,#5747,.F.);
#7819=ORIENTED_EDGE('',*,*,#5759,.T.);
#7820=ORIENTED_EDGE('',*,*,#5760,.T.);
#7821=ORIENTED_EDGE('',*,*,#5761,.T.);
#7822=ORIENTED_EDGE('',*,*,#5762,.T.);
#7823=ORIENTED_EDGE('',*,*,#5763,.T.);
#7824=ORIENTED_EDGE('',*,*,#5731,.F.);
#7825=ORIENTED_EDGE('',*,*,#5732,.F.);
#7826=ORIENTED_EDGE('',*,*,#5764,.T.);
#7827=ORIENTED_EDGE('',*,*,#5751,.F.);
#7828=ORIENTED_EDGE('',*,*,#5756,.F.);
#7829=ORIENTED_EDGE('',*,*,#5755,.F.);
#7830=ORIENTED_EDGE('',*,*,#5752,.F.);
#7831=ORIENTED_EDGE('',*,*,#5764,.F.);
#7832=ORIENTED_EDGE('',*,*,#5762,.F.);
#7833=ORIENTED_EDGE('',*,*,#5763,.F.);
#7834=ORIENTED_EDGE('',*,*,#5765,.T.);
#7835=ORIENTED_EDGE('',*,*,#5725,.F.);
#7836=ORIENTED_EDGE('',*,*,#5730,.F.);
#7837=ORIENTED_EDGE('',*,*,#5729,.F.);
#7838=ORIENTED_EDGE('',*,*,#5726,.F.);
#7839=ORIENTED_EDGE('',*,*,#5765,.F.);
#7840=ORIENTED_EDGE('',*,*,#5766,.T.);
#7841=ORIENTED_EDGE('',*,*,#5767,.T.);
#7842=ORIENTED_EDGE('',*,*,#5748,.F.);
#7843=ORIENTED_EDGE('',*,*,#5758,.F.);
#7844=ORIENTED_EDGE('',*,*,#5757,.F.);
#7845=ORIENTED_EDGE('',*,*,#5749,.F.);
#7846=ORIENTED_EDGE('',*,*,#5767,.F.);
#7847=ORIENTED_EDGE('',*,*,#5768,.T.);
#7848=ORIENTED_EDGE('',*,*,#5760,.F.);
#7849=ORIENTED_EDGE('',*,*,#5761,.F.);
#7850=ORIENTED_EDGE('',*,*,#5769,.T.);
#7851=ORIENTED_EDGE('',*,*,#5770,.T.);
#7852=ORIENTED_EDGE('',*,*,#5771,.T.);
#7853=ORIENTED_EDGE('',*,*,#5769,.F.);
#7854=ORIENTED_EDGE('',*,*,#5738,.T.);
#7855=ORIENTED_EDGE('',*,*,#5772,.T.);
#7856=ORIENTED_EDGE('',*,*,#5677,.T.);
#7857=ORIENTED_EDGE('',*,*,#5772,.F.);
#7858=ORIENTED_EDGE('',*,*,#5683,.T.);
#7859=ORIENTED_EDGE('',*,*,#5773,.T.);
#7860=ORIENTED_EDGE('',*,*,#5723,.T.);
#7861=ORIENTED_EDGE('',*,*,#5773,.F.);
#7862=ORIENTED_EDGE('',*,*,#5774,.F.);
#7863=ORIENTED_EDGE('',*,*,#5703,.T.);
#7864=ORIENTED_EDGE('',*,*,#5704,.T.);
#7865=ORIENTED_EDGE('',*,*,#5774,.T.);
#7866=ORIENTED_EDGE('',*,*,#5706,.T.);
#7867=ORIENTED_EDGE('',*,*,#5775,.F.);
#7868=ORIENTED_EDGE('',*,*,#5775,.T.);
#7869=ORIENTED_EDGE('',*,*,#5705,.T.);
#7870=ORIENTED_EDGE('',*,*,#5776,.F.);
#7871=ORIENTED_EDGE('',*,*,#5707,.T.);
#7872=ORIENTED_EDGE('',*,*,#5708,.T.);
#7873=ORIENTED_EDGE('',*,*,#5776,.T.);
#7874=ORIENTED_EDGE('',*,*,#5710,.T.);
#7875=ORIENTED_EDGE('',*,*,#5777,.F.);
#7876=ORIENTED_EDGE('',*,*,#5777,.T.);
#7877=ORIENTED_EDGE('',*,*,#5709,.T.);
#7878=ORIENTED_EDGE('',*,*,#5778,.F.);
#7879=ORIENTED_EDGE('',*,*,#5699,.T.);
#7880=ORIENTED_EDGE('',*,*,#5700,.T.);
#7881=ORIENTED_EDGE('',*,*,#5778,.T.);
#7882=ORIENTED_EDGE('',*,*,#5702,.T.);
#7883=ORIENTED_EDGE('',*,*,#5779,.F.);
#7884=ORIENTED_EDGE('',*,*,#5779,.T.);
#7885=ORIENTED_EDGE('',*,*,#5701,.T.);
#7886=ORIENTED_EDGE('',*,*,#5780,.F.);
#7887=ORIENTED_EDGE('',*,*,#5711,.T.);
#7888=ORIENTED_EDGE('',*,*,#5712,.T.);
#7889=ORIENTED_EDGE('',*,*,#5780,.T.);
#7890=ORIENTED_EDGE('',*,*,#5714,.T.);
#7891=ORIENTED_EDGE('',*,*,#5781,.F.);
#7892=ORIENTED_EDGE('',*,*,#5781,.T.);
#7893=ORIENTED_EDGE('',*,*,#5713,.T.);
#7894=ORIENTED_EDGE('',*,*,#5782,.F.);
#7895=ORIENTED_EDGE('',*,*,#5695,.T.);
#7896=ORIENTED_EDGE('',*,*,#5696,.T.);
#7897=ORIENTED_EDGE('',*,*,#5782,.T.);
#7898=ORIENTED_EDGE('',*,*,#5698,.T.);
#7899=ORIENTED_EDGE('',*,*,#5783,.F.);
#7900=ORIENTED_EDGE('',*,*,#5783,.T.);
#7901=ORIENTED_EDGE('',*,*,#5697,.T.);
#7902=ORIENTED_EDGE('',*,*,#5784,.F.);
#7903=ORIENTED_EDGE('',*,*,#5679,.T.);
#7904=ORIENTED_EDGE('',*,*,#5686,.T.);
#7905=ORIENTED_EDGE('',*,*,#5680,.T.);
#7906=ORIENTED_EDGE('',*,*,#5784,.T.);
#7907=ORIENTED_EDGE('',*,*,#5685,.T.);
#7908=ORIENTED_EDGE('',*,*,#5785,.F.);
#7909=ORIENTED_EDGE('',*,*,#5785,.T.);
#7910=ORIENTED_EDGE('',*,*,#5684,.T.);
#7911=ORIENTED_EDGE('',*,*,#5681,.T.);
#7912=ORIENTED_EDGE('',*,*,#5786,.F.);
#7913=ORIENTED_EDGE('',*,*,#5691,.T.);
#7914=ORIENTED_EDGE('',*,*,#5692,.T.);
#7915=ORIENTED_EDGE('',*,*,#5786,.T.);
#7916=ORIENTED_EDGE('',*,*,#5694,.T.);
#7917=ORIENTED_EDGE('',*,*,#5787,.F.);
#7918=ORIENTED_EDGE('',*,*,#5787,.T.);
#7919=ORIENTED_EDGE('',*,*,#5693,.T.);
#7920=ORIENTED_EDGE('',*,*,#5788,.F.);
#7921=ORIENTED_EDGE('',*,*,#5715,.T.);
#7922=ORIENTED_EDGE('',*,*,#5716,.T.);
#7923=ORIENTED_EDGE('',*,*,#5788,.T.);
#7924=ORIENTED_EDGE('',*,*,#5718,.T.);
#7925=ORIENTED_EDGE('',*,*,#5789,.F.);
#7926=ORIENTED_EDGE('',*,*,#5789,.T.);
#7927=ORIENTED_EDGE('',*,*,#5717,.T.);
#7928=ORIENTED_EDGE('',*,*,#5790,.F.);
#7929=ORIENTED_EDGE('',*,*,#5687,.T.);
#7930=ORIENTED_EDGE('',*,*,#5688,.T.);
#7931=ORIENTED_EDGE('',*,*,#5790,.T.);
#7932=ORIENTED_EDGE('',*,*,#5690,.T.);
#7933=ORIENTED_EDGE('',*,*,#5791,.F.);
#7934=ORIENTED_EDGE('',*,*,#5791,.T.);
#7935=ORIENTED_EDGE('',*,*,#5689,.T.);
#7936=ORIENTED_EDGE('',*,*,#5792,.F.);
#7937=ORIENTED_EDGE('',*,*,#5719,.T.);
#7938=ORIENTED_EDGE('',*,*,#5720,.T.);
#7939=ORIENTED_EDGE('',*,*,#5792,.T.);
#7940=ORIENTED_EDGE('',*,*,#5722,.T.);
#7941=ORIENTED_EDGE('',*,*,#5793,.F.);
#7942=ORIENTED_EDGE('',*,*,#5793,.T.);
#7943=ORIENTED_EDGE('',*,*,#5721,.T.);
#7944=ORIENTED_EDGE('',*,*,#5771,.F.);
#7945=ORIENTED_EDGE('',*,*,#5794,.T.);
#7946=ORIENTED_EDGE('',*,*,#5739,.F.);
#7947=ORIENTED_EDGE('',*,*,#5736,.F.);
#7948=ORIENTED_EDGE('',*,*,#5740,.F.);
#7949=ORIENTED_EDGE('',*,*,#5794,.F.);
#7950=ORIENTED_EDGE('',*,*,#5770,.F.);
#7951=ORIENTED_EDGE('',*,*,#5766,.F.);
#7952=ORIENTED_EDGE('',*,*,#5795,.T.);
#7953=ORIENTED_EDGE('',*,*,#5741,.F.);
#7954=ORIENTED_EDGE('',*,*,#5795,.F.);
#7955=ORIENTED_EDGE('',*,*,#5768,.F.);
#7956=ORIENTED_EDGE('',*,*,#5754,.F.);
#7957=ORIENTED_EDGE('',*,*,#5796,.T.);
#7958=ORIENTED_EDGE('',*,*,#5743,.F.);
#7959=ORIENTED_EDGE('',*,*,#5796,.F.);
#7960=ORIENTED_EDGE('',*,*,#5746,.F.);
#7961=ORIENTED_EDGE('',*,*,#5797,.T.);
#7962=ORIENTED_EDGE('',*,*,#5745,.F.);
#7963=ORIENTED_EDGE('',*,*,#5797,.F.);
#7964=ORIENTED_EDGE('',*,*,#5759,.F.);
#7965=ORIENTED_EDGE('',*,*,#5728,.F.);
#7966=ORIENTED_EDGE('',*,*,#5798,.T.);
#7967=ORIENTED_EDGE('',*,*,#5742,.F.);
#7968=ORIENTED_EDGE('',*,*,#5798,.F.);
#7969=ORIENTED_EDGE('',*,*,#5733,.F.);
#7970=ORIENTED_EDGE('',*,*,#5734,.F.);
#7971=ORIENTED_EDGE('',*,*,#5799,.T.);
#7972=ORIENTED_EDGE('',*,*,#5744,.F.);
#7973=ORIENTED_EDGE('',*,*,#5799,.F.);
#7974=ORIENTED_EDGE('',*,*,#5800,.T.);
#7975=ORIENTED_EDGE('',*,*,#5801,.T.);
#7976=ORIENTED_EDGE('',*,*,#5802,.T.);
#7977=ORIENTED_EDGE('',*,*,#5803,.T.);
#7978=ORIENTED_EDGE('',*,*,#5804,.T.);
#7979=ORIENTED_EDGE('',*,*,#5805,.F.);
#7980=ORIENTED_EDGE('',*,*,#5804,.F.);
#7981=ORIENTED_EDGE('',*,*,#5806,.T.);
#7982=ORIENTED_EDGE('',*,*,#5807,.T.);
#7983=ORIENTED_EDGE('',*,*,#5801,.F.);
#7984=ORIENTED_EDGE('',*,*,#5808,.F.);
#7985=ORIENTED_EDGE('',*,*,#5809,.F.);
#7986=ORIENTED_EDGE('',*,*,#5805,.T.);
#7987=ORIENTED_EDGE('',*,*,#5810,.F.);
#7988=ORIENTED_EDGE('',*,*,#5800,.F.);
#7989=ORIENTED_EDGE('',*,*,#5811,.F.);
#7990=ORIENTED_EDGE('',*,*,#5812,.F.);
#7991=ORIENTED_EDGE('',*,*,#5813,.T.);
#7992=ORIENTED_EDGE('',*,*,#5802,.F.);
#7993=ORIENTED_EDGE('',*,*,#5807,.F.);
#7994=ORIENTED_EDGE('',*,*,#5806,.F.);
#7995=ORIENTED_EDGE('',*,*,#5803,.F.);
#7996=ORIENTED_EDGE('',*,*,#5813,.F.);
#7997=ORIENTED_EDGE('',*,*,#5812,.T.);
#7998=ORIENTED_EDGE('',*,*,#5814,.T.);
#7999=ORIENTED_EDGE('',*,*,#5815,.T.);
#8000=ORIENTED_EDGE('',*,*,#5809,.T.);
#8001=ORIENTED_EDGE('',*,*,#5808,.T.);
#8002=ORIENTED_EDGE('',*,*,#5815,.F.);
#8003=ORIENTED_EDGE('',*,*,#5814,.F.);
#8004=ORIENTED_EDGE('',*,*,#5810,.T.);
#8005=ORIENTED_EDGE('',*,*,#5816,.T.);
#8006=ORIENTED_EDGE('',*,*,#5811,.T.);
#8007=ORIENTED_EDGE('',*,*,#5816,.F.);
#8008=ORIENTED_EDGE('',*,*,#5817,.T.);
#8009=ORIENTED_EDGE('',*,*,#5818,.T.);
#8010=ORIENTED_EDGE('',*,*,#5817,.F.);
#8011=ORIENTED_EDGE('',*,*,#5819,.T.);
#8012=ORIENTED_EDGE('',*,*,#5820,.T.);
#8013=ORIENTED_EDGE('',*,*,#5819,.F.);
#8014=ORIENTED_EDGE('',*,*,#5821,.T.);
#8015=ORIENTED_EDGE('',*,*,#5822,.T.);
#8016=ORIENTED_EDGE('',*,*,#5822,.F.);
#8017=ORIENTED_EDGE('',*,*,#5823,.F.);
#8018=ORIENTED_EDGE('',*,*,#5823,.T.);
#8019=ORIENTED_EDGE('',*,*,#5820,.F.);
#8020=ORIENTED_EDGE('',*,*,#5824,.T.);
#8021=ORIENTED_EDGE('',*,*,#5821,.F.);
#8022=ORIENTED_EDGE('',*,*,#5824,.F.);
#8023=ORIENTED_EDGE('',*,*,#5818,.F.);
#8024=ORIENTED_EDGE('',*,*,#5825,.T.);
#8025=ORIENTED_EDGE('',*,*,#5826,.T.);
#8026=ORIENTED_EDGE('',*,*,#5825,.F.);
#8027=ORIENTED_EDGE('',*,*,#5826,.F.);
#8028=ORIENTED_EDGE('',*,*,#5827,.T.);
#8029=ORIENTED_EDGE('',*,*,#5828,.T.);
#8030=ORIENTED_EDGE('',*,*,#5827,.F.);
#8031=ORIENTED_EDGE('',*,*,#5829,.T.);
#8032=ORIENTED_EDGE('',*,*,#5830,.T.);
#8033=ORIENTED_EDGE('',*,*,#5831,.T.);
#8034=ORIENTED_EDGE('',*,*,#5832,.T.);
#8035=ORIENTED_EDGE('',*,*,#5833,.T.);
#8036=ORIENTED_EDGE('',*,*,#5834,.T.);
#8037=ORIENTED_EDGE('',*,*,#5835,.T.);
#8038=ORIENTED_EDGE('',*,*,#5836,.F.);
#8039=ORIENTED_EDGE('',*,*,#5831,.F.);
#8040=ORIENTED_EDGE('',*,*,#5837,.T.);
#8041=ORIENTED_EDGE('',*,*,#5838,.T.);
#8042=ORIENTED_EDGE('',*,*,#5839,.F.);
#8043=ORIENTED_EDGE('',*,*,#5832,.F.);
#8044=ORIENTED_EDGE('',*,*,#5836,.T.);
#8045=ORIENTED_EDGE('',*,*,#5840,.T.);
#8046=ORIENTED_EDGE('',*,*,#5841,.F.);
#8047=ORIENTED_EDGE('',*,*,#5833,.F.);
#8048=ORIENTED_EDGE('',*,*,#5839,.T.);
#8049=ORIENTED_EDGE('',*,*,#5842,.T.);
#8050=ORIENTED_EDGE('',*,*,#5843,.F.);
#8051=ORIENTED_EDGE('',*,*,#5834,.F.);
#8052=ORIENTED_EDGE('',*,*,#5841,.T.);
#8053=ORIENTED_EDGE('',*,*,#5844,.T.);
#8054=ORIENTED_EDGE('',*,*,#5845,.F.);
#8055=ORIENTED_EDGE('',*,*,#5829,.F.);
#8056=ORIENTED_EDGE('',*,*,#5843,.T.);
#8057=ORIENTED_EDGE('',*,*,#5846,.T.);
#8058=ORIENTED_EDGE('',*,*,#5837,.F.);
#8059=ORIENTED_EDGE('',*,*,#5830,.F.);
#8060=ORIENTED_EDGE('',*,*,#5845,.T.);
#8061=ORIENTED_EDGE('',*,*,#5828,.F.);
#8062=ORIENTED_EDGE('',*,*,#5846,.F.);
#8063=ORIENTED_EDGE('',*,*,#5844,.F.);
#8064=ORIENTED_EDGE('',*,*,#5842,.F.);
#8065=ORIENTED_EDGE('',*,*,#5840,.F.);
#8066=ORIENTED_EDGE('',*,*,#5838,.F.);
#8067=ORIENTED_EDGE('',*,*,#5835,.F.);
#8068=ORIENTED_EDGE('',*,*,#5847,.T.);
#8069=ORIENTED_EDGE('',*,*,#5848,.T.);
#8070=ORIENTED_EDGE('',*,*,#5849,.F.);
#8071=ORIENTED_EDGE('',*,*,#5850,.T.);
#8072=ORIENTED_EDGE('',*,*,#5847,.F.);
#8073=ORIENTED_EDGE('',*,*,#5851,.T.);
#8074=ORIENTED_EDGE('',*,*,#5852,.T.);
#8075=ORIENTED_EDGE('',*,*,#5850,.F.);
#8076=ORIENTED_EDGE('',*,*,#5851,.F.);
#8077=ORIENTED_EDGE('',*,*,#5853,.T.);
#8078=ORIENTED_EDGE('',*,*,#5853,.F.);
#8079=ORIENTED_EDGE('',*,*,#5848,.F.);
#8080=ORIENTED_EDGE('',*,*,#5849,.T.);
#8081=ORIENTED_EDGE('',*,*,#5852,.F.);
#8082=ORIENTED_EDGE('',*,*,#5854,.T.);
#8083=ORIENTED_EDGE('',*,*,#5855,.T.);
#8084=ORIENTED_EDGE('',*,*,#5856,.T.);
#8085=ORIENTED_EDGE('',*,*,#5857,.F.);
#8086=ORIENTED_EDGE('',*,*,#5856,.F.);
#8087=ORIENTED_EDGE('',*,*,#5857,.T.);
#8088=ORIENTED_EDGE('',*,*,#5858,.F.);
#8089=ORIENTED_EDGE('',*,*,#5859,.T.);
#8090=ORIENTED_EDGE('',*,*,#5860,.F.);
#8091=ORIENTED_EDGE('',*,*,#5858,.T.);
#8092=ORIENTED_EDGE('',*,*,#5861,.T.);
#8093=ORIENTED_EDGE('',*,*,#5862,.F.);
#8094=ORIENTED_EDGE('',*,*,#5861,.F.);
#8095=ORIENTED_EDGE('',*,*,#5862,.T.);
#8096=ORIENTED_EDGE('',*,*,#5863,.F.);
#8097=ORIENTED_EDGE('',*,*,#5864,.F.);
#8098=ORIENTED_EDGE('',*,*,#5865,.F.);
#8099=ORIENTED_EDGE('',*,*,#5866,.F.);
#8100=ORIENTED_EDGE('',*,*,#5863,.T.);
#8101=ORIENTED_EDGE('',*,*,#5867,.F.);
#8102=ORIENTED_EDGE('',*,*,#5868,.F.);
#8103=ORIENTED_EDGE('',*,*,#5869,.T.);
#8104=ORIENTED_EDGE('',*,*,#5864,.T.);
#8105=ORIENTED_EDGE('',*,*,#5869,.F.);
#8106=ORIENTED_EDGE('',*,*,#5870,.F.);
#8107=ORIENTED_EDGE('',*,*,#5871,.T.);
#8108=ORIENTED_EDGE('',*,*,#5865,.T.);
#8109=ORIENTED_EDGE('',*,*,#5871,.F.);
#8110=ORIENTED_EDGE('',*,*,#5872,.F.);
#8111=ORIENTED_EDGE('',*,*,#5873,.T.);
#8112=ORIENTED_EDGE('',*,*,#5866,.T.);
#8113=ORIENTED_EDGE('',*,*,#5873,.F.);
#8114=ORIENTED_EDGE('',*,*,#5874,.F.);
#8115=ORIENTED_EDGE('',*,*,#5867,.T.);
#8116=ORIENTED_EDGE('',*,*,#5868,.T.);
#8117=ORIENTED_EDGE('',*,*,#5874,.T.);
#8118=ORIENTED_EDGE('',*,*,#5872,.T.);
#8119=ORIENTED_EDGE('',*,*,#5870,.T.);
#8120=ORIENTED_EDGE('',*,*,#5854,.F.);
#8121=ORIENTED_EDGE('',*,*,#5855,.F.);
#8122=ORIENTED_EDGE('',*,*,#5875,.T.);
#8123=ORIENTED_EDGE('',*,*,#5859,.F.);
#8124=ORIENTED_EDGE('',*,*,#5875,.F.);
#8125=ORIENTED_EDGE('',*,*,#5860,.T.);
#8126=ORIENTED_EDGE('',*,*,#5876,.T.);
#8127=ORIENTED_EDGE('',*,*,#5877,.T.);
#8128=ORIENTED_EDGE('',*,*,#5878,.T.);
#8129=ORIENTED_EDGE('',*,*,#5879,.T.);
#8130=ORIENTED_EDGE('',*,*,#5880,.T.);
#8131=ORIENTED_EDGE('',*,*,#5881,.T.);
#8132=ORIENTED_EDGE('',*,*,#5882,.T.);
#8133=ORIENTED_EDGE('',*,*,#5883,.T.);
#8134=ORIENTED_EDGE('',*,*,#5884,.T.);
#8135=ORIENTED_EDGE('',*,*,#5885,.T.);
#8136=ORIENTED_EDGE('',*,*,#5886,.T.);
#8137=ORIENTED_EDGE('',*,*,#5887,.T.);
#8138=ORIENTED_EDGE('',*,*,#5888,.T.);
#8139=ORIENTED_EDGE('',*,*,#5889,.T.);
#8140=ORIENTED_EDGE('',*,*,#5890,.T.);
#8141=ORIENTED_EDGE('',*,*,#5891,.T.);
#8142=ORIENTED_EDGE('',*,*,#5892,.T.);
#8143=ORIENTED_EDGE('',*,*,#5893,.F.);
#8144=ORIENTED_EDGE('',*,*,#5876,.F.);
#8145=ORIENTED_EDGE('',*,*,#5894,.T.);
#8146=ORIENTED_EDGE('',*,*,#5895,.T.);
#8147=ORIENTED_EDGE('',*,*,#5896,.F.);
#8148=ORIENTED_EDGE('',*,*,#5877,.F.);
#8149=ORIENTED_EDGE('',*,*,#5893,.T.);
#8150=ORIENTED_EDGE('',*,*,#5897,.T.);
#8151=ORIENTED_EDGE('',*,*,#5898,.F.);
#8152=ORIENTED_EDGE('',*,*,#5878,.F.);
#8153=ORIENTED_EDGE('',*,*,#5896,.T.);
#8154=ORIENTED_EDGE('',*,*,#5899,.T.);
#8155=ORIENTED_EDGE('',*,*,#5894,.F.);
#8156=ORIENTED_EDGE('',*,*,#5879,.F.);
#8157=ORIENTED_EDGE('',*,*,#5898,.T.);
#8158=ORIENTED_EDGE('',*,*,#5892,.F.);
#8159=ORIENTED_EDGE('',*,*,#5899,.F.);
#8160=ORIENTED_EDGE('',*,*,#5897,.F.);
#8161=ORIENTED_EDGE('',*,*,#5895,.F.);
#8162=ORIENTED_EDGE('',*,*,#5900,.F.);
#8163=ORIENTED_EDGE('',*,*,#5901,.F.);
#8164=ORIENTED_EDGE('',*,*,#5902,.F.);
#8165=ORIENTED_EDGE('',*,*,#5903,.F.);
#8166=ORIENTED_EDGE('',*,*,#5904,.F.);
#8167=ORIENTED_EDGE('',*,*,#5905,.F.);
#8168=ORIENTED_EDGE('',*,*,#5906,.F.);
#8169=ORIENTED_EDGE('',*,*,#5907,.F.);
#8170=ORIENTED_EDGE('',*,*,#5908,.F.);
#8171=ORIENTED_EDGE('',*,*,#5909,.F.);
#8172=ORIENTED_EDGE('',*,*,#5910,.F.);
#8173=ORIENTED_EDGE('',*,*,#5911,.F.);
#8174=ORIENTED_EDGE('',*,*,#5880,.F.);
#8175=ORIENTED_EDGE('',*,*,#5912,.F.);
#8176=ORIENTED_EDGE('',*,*,#5913,.T.);
#8177=ORIENTED_EDGE('',*,*,#5914,.T.);
#8178=ORIENTED_EDGE('',*,*,#5881,.F.);
#8179=ORIENTED_EDGE('',*,*,#5914,.F.);
#8180=ORIENTED_EDGE('',*,*,#5915,.T.);
#8181=ORIENTED_EDGE('',*,*,#5916,.T.);
#8182=ORIENTED_EDGE('',*,*,#5882,.F.);
#8183=ORIENTED_EDGE('',*,*,#5916,.F.);
#8184=ORIENTED_EDGE('',*,*,#5917,.T.);
#8185=ORIENTED_EDGE('',*,*,#5918,.T.);
#8186=ORIENTED_EDGE('',*,*,#5883,.F.);
#8187=ORIENTED_EDGE('',*,*,#5918,.F.);
#8188=ORIENTED_EDGE('',*,*,#5919,.T.);
#8189=ORIENTED_EDGE('',*,*,#5920,.T.);
#8190=ORIENTED_EDGE('',*,*,#5884,.F.);
#8191=ORIENTED_EDGE('',*,*,#5920,.F.);
#8192=ORIENTED_EDGE('',*,*,#5921,.T.);
#8193=ORIENTED_EDGE('',*,*,#5922,.T.);
#8194=ORIENTED_EDGE('',*,*,#5885,.F.);
#8195=ORIENTED_EDGE('',*,*,#5922,.F.);
#8196=ORIENTED_EDGE('',*,*,#5923,.T.);
#8197=ORIENTED_EDGE('',*,*,#5924,.T.);
#8198=ORIENTED_EDGE('',*,*,#5886,.F.);
#8199=ORIENTED_EDGE('',*,*,#5924,.F.);
#8200=ORIENTED_EDGE('',*,*,#5925,.T.);
#8201=ORIENTED_EDGE('',*,*,#5926,.T.);
#8202=ORIENTED_EDGE('',*,*,#5887,.F.);
#8203=ORIENTED_EDGE('',*,*,#5926,.F.);
#8204=ORIENTED_EDGE('',*,*,#5927,.T.);
#8205=ORIENTED_EDGE('',*,*,#5928,.T.);
#8206=ORIENTED_EDGE('',*,*,#5888,.F.);
#8207=ORIENTED_EDGE('',*,*,#5928,.F.);
#8208=ORIENTED_EDGE('',*,*,#5929,.T.);
#8209=ORIENTED_EDGE('',*,*,#5930,.T.);
#8210=ORIENTED_EDGE('',*,*,#5889,.F.);
#8211=ORIENTED_EDGE('',*,*,#5930,.F.);
#8212=ORIENTED_EDGE('',*,*,#5931,.T.);
#8213=ORIENTED_EDGE('',*,*,#5932,.T.);
#8214=ORIENTED_EDGE('',*,*,#5890,.F.);
#8215=ORIENTED_EDGE('',*,*,#5932,.F.);
#8216=ORIENTED_EDGE('',*,*,#5933,.T.);
#8217=ORIENTED_EDGE('',*,*,#5934,.T.);
#8218=ORIENTED_EDGE('',*,*,#5891,.F.);
#8219=ORIENTED_EDGE('',*,*,#5934,.F.);
#8220=ORIENTED_EDGE('',*,*,#5935,.T.);
#8221=ORIENTED_EDGE('',*,*,#5912,.T.);
#8222=ORIENTED_EDGE('',*,*,#5913,.F.);
#8223=ORIENTED_EDGE('',*,*,#5935,.F.);
#8224=ORIENTED_EDGE('',*,*,#5933,.F.);
#8225=ORIENTED_EDGE('',*,*,#5931,.F.);
#8226=ORIENTED_EDGE('',*,*,#5929,.F.);
#8227=ORIENTED_EDGE('',*,*,#5927,.F.);
#8228=ORIENTED_EDGE('',*,*,#5925,.F.);
#8229=ORIENTED_EDGE('',*,*,#5923,.F.);
#8230=ORIENTED_EDGE('',*,*,#5921,.F.);
#8231=ORIENTED_EDGE('',*,*,#5919,.F.);
#8232=ORIENTED_EDGE('',*,*,#5917,.F.);
#8233=ORIENTED_EDGE('',*,*,#5915,.F.);
#8234=ORIENTED_EDGE('',*,*,#5900,.T.);
#8235=ORIENTED_EDGE('',*,*,#5936,.F.);
#8236=ORIENTED_EDGE('',*,*,#5937,.F.);
#8237=ORIENTED_EDGE('',*,*,#5938,.T.);
#8238=ORIENTED_EDGE('',*,*,#5901,.T.);
#8239=ORIENTED_EDGE('',*,*,#5938,.F.);
#8240=ORIENTED_EDGE('',*,*,#5939,.F.);
#8241=ORIENTED_EDGE('',*,*,#5940,.T.);
#8242=ORIENTED_EDGE('',*,*,#5902,.T.);
#8243=ORIENTED_EDGE('',*,*,#5940,.F.);
#8244=ORIENTED_EDGE('',*,*,#5941,.F.);
#8245=ORIENTED_EDGE('',*,*,#5942,.T.);
#8246=ORIENTED_EDGE('',*,*,#5903,.T.);
#8247=ORIENTED_EDGE('',*,*,#5942,.F.);
#8248=ORIENTED_EDGE('',*,*,#5943,.F.);
#8249=ORIENTED_EDGE('',*,*,#5944,.T.);
#8250=ORIENTED_EDGE('',*,*,#5904,.T.);
#8251=ORIENTED_EDGE('',*,*,#5944,.F.);
#8252=ORIENTED_EDGE('',*,*,#5945,.F.);
#8253=ORIENTED_EDGE('',*,*,#5946,.T.);
#8254=ORIENTED_EDGE('',*,*,#5905,.T.);
#8255=ORIENTED_EDGE('',*,*,#5946,.F.);
#8256=ORIENTED_EDGE('',*,*,#5947,.F.);
#8257=ORIENTED_EDGE('',*,*,#5948,.T.);
#8258=ORIENTED_EDGE('',*,*,#5906,.T.);
#8259=ORIENTED_EDGE('',*,*,#5948,.F.);
#8260=ORIENTED_EDGE('',*,*,#5949,.F.);
#8261=ORIENTED_EDGE('',*,*,#5950,.T.);
#8262=ORIENTED_EDGE('',*,*,#5907,.T.);
#8263=ORIENTED_EDGE('',*,*,#5950,.F.);
#8264=ORIENTED_EDGE('',*,*,#5951,.F.);
#8265=ORIENTED_EDGE('',*,*,#5952,.T.);
#8266=ORIENTED_EDGE('',*,*,#5908,.T.);
#8267=ORIENTED_EDGE('',*,*,#5952,.F.);
#8268=ORIENTED_EDGE('',*,*,#5953,.F.);
#8269=ORIENTED_EDGE('',*,*,#5954,.T.);
#8270=ORIENTED_EDGE('',*,*,#5909,.T.);
#8271=ORIENTED_EDGE('',*,*,#5954,.F.);
#8272=ORIENTED_EDGE('',*,*,#5955,.F.);
#8273=ORIENTED_EDGE('',*,*,#5956,.T.);
#8274=ORIENTED_EDGE('',*,*,#5910,.T.);
#8275=ORIENTED_EDGE('',*,*,#5956,.F.);
#8276=ORIENTED_EDGE('',*,*,#5957,.F.);
#8277=ORIENTED_EDGE('',*,*,#5958,.T.);
#8278=ORIENTED_EDGE('',*,*,#5911,.T.);
#8279=ORIENTED_EDGE('',*,*,#5958,.F.);
#8280=ORIENTED_EDGE('',*,*,#5959,.F.);
#8281=ORIENTED_EDGE('',*,*,#5936,.T.);
#8282=ORIENTED_EDGE('',*,*,#5937,.T.);
#8283=ORIENTED_EDGE('',*,*,#5959,.T.);
#8284=ORIENTED_EDGE('',*,*,#5957,.T.);
#8285=ORIENTED_EDGE('',*,*,#5955,.T.);
#8286=ORIENTED_EDGE('',*,*,#5953,.T.);
#8287=ORIENTED_EDGE('',*,*,#5951,.T.);
#8288=ORIENTED_EDGE('',*,*,#5949,.T.);
#8289=ORIENTED_EDGE('',*,*,#5947,.T.);
#8290=ORIENTED_EDGE('',*,*,#5945,.T.);
#8291=ORIENTED_EDGE('',*,*,#5943,.T.);
#8292=ORIENTED_EDGE('',*,*,#5941,.T.);
#8293=ORIENTED_EDGE('',*,*,#5939,.T.);
#8294=ORIENTED_EDGE('',*,*,#5960,.T.);
#8295=ORIENTED_EDGE('',*,*,#5961,.T.);
#8296=ORIENTED_EDGE('',*,*,#5962,.F.);
#8297=ORIENTED_EDGE('',*,*,#5961,.F.);
#8298=ORIENTED_EDGE('',*,*,#5962,.T.);
#8299=ORIENTED_EDGE('',*,*,#5960,.F.);
#8300=ORIENTED_EDGE('',*,*,#5963,.T.);
#8301=ORIENTED_EDGE('',*,*,#5964,.T.);
#8302=ORIENTED_EDGE('',*,*,#5965,.F.);
#8303=ORIENTED_EDGE('',*,*,#5964,.F.);
#8304=ORIENTED_EDGE('',*,*,#5965,.T.);
#8305=ORIENTED_EDGE('',*,*,#5963,.F.);
#8306=ORIENTED_EDGE('',*,*,#5966,.T.);
#8307=ORIENTED_EDGE('',*,*,#5967,.F.);
#8308=ORIENTED_EDGE('',*,*,#5968,.F.);
#8309=ORIENTED_EDGE('',*,*,#5969,.T.);
#8310=ORIENTED_EDGE('',*,*,#5968,.T.);
#8311=ORIENTED_EDGE('',*,*,#5970,.T.);
#8312=ORIENTED_EDGE('',*,*,#5966,.F.);
#8313=ORIENTED_EDGE('',*,*,#5970,.F.);
#8314=ORIENTED_EDGE('',*,*,#5967,.T.);
#8315=ORIENTED_EDGE('',*,*,#5971,.T.);
#8316=ORIENTED_EDGE('',*,*,#5969,.F.);
#8317=ORIENTED_EDGE('',*,*,#5971,.F.);
#8318=ORIENTED_EDGE('',*,*,#5972,.F.);
#8319=ORIENTED_EDGE('',*,*,#5973,.T.);
#8320=ORIENTED_EDGE('',*,*,#5974,.T.);
#8321=ORIENTED_EDGE('',*,*,#5973,.F.);
#8322=ORIENTED_EDGE('',*,*,#5975,.T.);
#8323=ORIENTED_EDGE('',*,*,#5974,.F.);
#8324=ORIENTED_EDGE('',*,*,#5975,.F.);
#8325=ORIENTED_EDGE('',*,*,#5976,.T.);
#8326=ORIENTED_EDGE('',*,*,#5977,.T.);
#8327=ORIENTED_EDGE('',*,*,#5976,.F.);
#8328=ORIENTED_EDGE('',*,*,#5977,.F.);
#8329=ORIENTED_EDGE('',*,*,#5978,.F.);
#8330=ORIENTED_EDGE('',*,*,#5979,.T.);
#8331=ORIENTED_EDGE('',*,*,#5979,.F.);
#8332=ORIENTED_EDGE('',*,*,#5980,.T.);
#8333=ORIENTED_EDGE('',*,*,#5981,.T.);
#8334=ORIENTED_EDGE('',*,*,#5980,.F.);
#8335=ORIENTED_EDGE('',*,*,#5972,.T.);
#8336=ORIENTED_EDGE('',*,*,#5981,.F.);
#8337=ORIENTED_EDGE('',*,*,#5982,.T.);
#8338=ORIENTED_EDGE('',*,*,#5982,.F.);
#8339=ORIENTED_EDGE('',*,*,#5983,.T.);
#8340=ORIENTED_EDGE('',*,*,#5978,.T.);
#8341=ORIENTED_EDGE('',*,*,#5983,.F.);
#8342=ORIENTED_EDGE('',*,*,#5984,.T.);
#8343=ORIENTED_EDGE('',*,*,#5985,.T.);
#8344=ORIENTED_EDGE('',*,*,#5986,.T.);
#8345=ORIENTED_EDGE('',*,*,#5987,.T.);
#8346=ORIENTED_EDGE('',*,*,#5988,.T.);
#8347=ORIENTED_EDGE('',*,*,#5989,.T.);
#8348=ORIENTED_EDGE('',*,*,#5990,.T.);
#8349=ORIENTED_EDGE('',*,*,#5991,.T.);
#8350=ORIENTED_EDGE('',*,*,#5992,.T.);
#8351=ORIENTED_EDGE('',*,*,#5993,.T.);
#8352=ORIENTED_EDGE('',*,*,#5994,.T.);
#8353=ORIENTED_EDGE('',*,*,#5995,.T.);
#8354=ORIENTED_EDGE('',*,*,#5996,.T.);
#8355=ORIENTED_EDGE('',*,*,#5997,.T.);
#8356=ORIENTED_EDGE('',*,*,#5998,.T.);
#8357=ORIENTED_EDGE('',*,*,#5999,.T.);
#8358=ORIENTED_EDGE('',*,*,#6000,.T.);
#8359=ORIENTED_EDGE('',*,*,#6001,.T.);
#8360=ORIENTED_EDGE('',*,*,#6002,.T.);
#8361=ORIENTED_EDGE('',*,*,#6003,.T.);
#8362=ORIENTED_EDGE('',*,*,#6004,.T.);
#8363=ORIENTED_EDGE('',*,*,#6005,.T.);
#8364=ORIENTED_EDGE('',*,*,#6006,.T.);
#8365=ORIENTED_EDGE('',*,*,#6007,.T.);
#8366=ORIENTED_EDGE('',*,*,#6008,.T.);
#8367=ORIENTED_EDGE('',*,*,#6009,.T.);
#8368=ORIENTED_EDGE('',*,*,#6010,.T.);
#8369=ORIENTED_EDGE('',*,*,#6011,.T.);
#8370=ORIENTED_EDGE('',*,*,#6012,.T.);
#8371=ORIENTED_EDGE('',*,*,#6013,.T.);
#8372=ORIENTED_EDGE('',*,*,#6014,.T.);
#8373=ORIENTED_EDGE('',*,*,#6015,.T.);
#8374=ORIENTED_EDGE('',*,*,#6016,.T.);
#8375=ORIENTED_EDGE('',*,*,#6017,.T.);
#8376=ORIENTED_EDGE('',*,*,#6018,.T.);
#8377=ORIENTED_EDGE('',*,*,#6019,.T.);
#8378=ORIENTED_EDGE('',*,*,#6020,.T.);
#8379=ORIENTED_EDGE('',*,*,#6021,.T.);
#8380=ORIENTED_EDGE('',*,*,#6022,.T.);
#8381=ORIENTED_EDGE('',*,*,#6023,.T.);
#8382=ORIENTED_EDGE('',*,*,#6024,.T.);
#8383=ORIENTED_EDGE('',*,*,#6025,.T.);
#8384=ORIENTED_EDGE('',*,*,#6026,.T.);
#8385=ORIENTED_EDGE('',*,*,#6027,.T.);
#8386=ORIENTED_EDGE('',*,*,#6028,.T.);
#8387=ORIENTED_EDGE('',*,*,#6029,.T.);
#8388=ORIENTED_EDGE('',*,*,#6030,.T.);
#8389=ORIENTED_EDGE('',*,*,#6031,.T.);
#8390=ORIENTED_EDGE('',*,*,#6032,.T.);
#8391=ORIENTED_EDGE('',*,*,#6033,.T.);
#8392=ORIENTED_EDGE('',*,*,#6034,.T.);
#8393=ORIENTED_EDGE('',*,*,#6035,.T.);
#8394=ORIENTED_EDGE('',*,*,#6036,.T.);
#8395=ORIENTED_EDGE('',*,*,#6037,.T.);
#8396=ORIENTED_EDGE('',*,*,#6038,.T.);
#8397=ORIENTED_EDGE('',*,*,#6039,.T.);
#8398=ORIENTED_EDGE('',*,*,#6040,.T.);
#8399=ORIENTED_EDGE('',*,*,#6041,.T.);
#8400=ORIENTED_EDGE('',*,*,#6042,.T.);
#8401=ORIENTED_EDGE('',*,*,#6043,.T.);
#8402=ORIENTED_EDGE('',*,*,#6044,.T.);
#8403=ORIENTED_EDGE('',*,*,#6045,.T.);
#8404=ORIENTED_EDGE('',*,*,#6046,.T.);
#8405=ORIENTED_EDGE('',*,*,#6047,.T.);
#8406=ORIENTED_EDGE('',*,*,#6048,.T.);
#8407=ORIENTED_EDGE('',*,*,#6049,.T.);
#8408=ORIENTED_EDGE('',*,*,#6050,.T.);
#8409=ORIENTED_EDGE('',*,*,#6051,.T.);
#8410=ORIENTED_EDGE('',*,*,#6052,.T.);
#8411=ORIENTED_EDGE('',*,*,#6053,.T.);
#8412=ORIENTED_EDGE('',*,*,#6054,.T.);
#8413=ORIENTED_EDGE('',*,*,#6055,.T.);
#8414=ORIENTED_EDGE('',*,*,#6056,.T.);
#8415=ORIENTED_EDGE('',*,*,#5994,.F.);
#8416=ORIENTED_EDGE('',*,*,#6057,.T.);
#8417=ORIENTED_EDGE('',*,*,#6002,.F.);
#8418=ORIENTED_EDGE('',*,*,#6058,.T.);
#8419=ORIENTED_EDGE('',*,*,#6010,.F.);
#8420=ORIENTED_EDGE('',*,*,#6059,.T.);
#8421=ORIENTED_EDGE('',*,*,#6017,.F.);
#8422=ORIENTED_EDGE('',*,*,#6060,.T.);
#8423=ORIENTED_EDGE('',*,*,#6027,.F.);
#8424=ORIENTED_EDGE('',*,*,#6061,.T.);
#8425=ORIENTED_EDGE('',*,*,#6035,.F.);
#8426=ORIENTED_EDGE('',*,*,#6062,.T.);
#8427=ORIENTED_EDGE('',*,*,#6043,.F.);
#8428=ORIENTED_EDGE('',*,*,#6063,.T.);
#8429=ORIENTED_EDGE('',*,*,#6051,.F.);
#8430=ORIENTED_EDGE('',*,*,#6064,.T.);
#8431=ORIENTED_EDGE('',*,*,#6065,.F.);
#8432=ORIENTED_EDGE('',*,*,#6066,.T.);
#8433=ORIENTED_EDGE('',*,*,#5984,.F.);
#8434=ORIENTED_EDGE('',*,*,#6067,.T.);
#8435=ORIENTED_EDGE('',*,*,#6068,.F.);
#8436=ORIENTED_EDGE('',*,*,#6069,.T.);
#8437=ORIENTED_EDGE('',*,*,#6070,.T.);
#8438=ORIENTED_EDGE('',*,*,#6071,.T.);
#8439=ORIENTED_EDGE('',*,*,#6070,.F.);
#8440=ORIENTED_EDGE('',*,*,#6072,.F.);
#8441=ORIENTED_EDGE('',*,*,#6073,.T.);
#8442=ORIENTED_EDGE('',*,*,#6074,.F.);
#8443=ORIENTED_EDGE('',*,*,#6073,.F.);
#8444=ORIENTED_EDGE('',*,*,#6075,.T.);
#8445=ORIENTED_EDGE('',*,*,#6076,.T.);
#8446=ORIENTED_EDGE('',*,*,#6065,.T.);
#8447=ORIENTED_EDGE('',*,*,#6077,.T.);
#8448=ORIENTED_EDGE('',*,*,#6078,.T.);
#8449=ORIENTED_EDGE('',*,*,#6079,.T.);
#8450=ORIENTED_EDGE('',*,*,#6080,.T.);
#8451=ORIENTED_EDGE('',*,*,#6081,.T.);
#8452=ORIENTED_EDGE('',*,*,#6082,.T.);
#8453=ORIENTED_EDGE('',*,*,#6083,.F.);
#8454=ORIENTED_EDGE('',*,*,#6084,.T.);
#8455=ORIENTED_EDGE('',*,*,#6085,.T.);
#8456=ORIENTED_EDGE('',*,*,#6086,.T.);
#8457=ORIENTED_EDGE('',*,*,#6082,.F.);
#8458=ORIENTED_EDGE('',*,*,#6086,.F.);
#8459=ORIENTED_EDGE('',*,*,#6084,.F.);
#8460=ORIENTED_EDGE('',*,*,#6085,.F.);
#8461=ORIENTED_EDGE('',*,*,#6087,.T.);
#8462=ORIENTED_EDGE('',*,*,#6088,.T.);
#8463=ORIENTED_EDGE('',*,*,#6087,.F.);
#8464=ORIENTED_EDGE('',*,*,#6089,.T.);
#8465=ORIENTED_EDGE('',*,*,#6090,.T.);
#8466=ORIENTED_EDGE('',*,*,#6091,.T.);
#8467=ORIENTED_EDGE('',*,*,#6092,.T.);
#8468=ORIENTED_EDGE('',*,*,#6093,.T.);
#8469=ORIENTED_EDGE('',*,*,#6094,.T.);
#8470=ORIENTED_EDGE('',*,*,#6095,.T.);
#8471=ORIENTED_EDGE('',*,*,#6096,.T.);
#8472=ORIENTED_EDGE('',*,*,#6097,.T.);
#8473=ORIENTED_EDGE('',*,*,#6098,.T.);
#8474=ORIENTED_EDGE('',*,*,#6099,.T.);
#8475=ORIENTED_EDGE('',*,*,#6088,.F.);
#8476=ORIENTED_EDGE('',*,*,#6099,.F.);
#8477=ORIENTED_EDGE('',*,*,#6100,.T.);
#8478=ORIENTED_EDGE('',*,*,#6101,.T.);
#8479=ORIENTED_EDGE('',*,*,#6102,.T.);
#8480=ORIENTED_EDGE('',*,*,#6100,.F.);
#8481=ORIENTED_EDGE('',*,*,#5988,.F.);
#8482=ORIENTED_EDGE('',*,*,#6103,.T.);
#8483=ORIENTED_EDGE('',*,*,#6080,.F.);
#8484=ORIENTED_EDGE('',*,*,#6104,.T.);
#8485=ORIENTED_EDGE('',*,*,#6055,.F.);
#8486=ORIENTED_EDGE('',*,*,#6105,.T.);
#8487=ORIENTED_EDGE('',*,*,#6047,.F.);
#8488=ORIENTED_EDGE('',*,*,#6106,.T.);
#8489=ORIENTED_EDGE('',*,*,#6039,.F.);
#8490=ORIENTED_EDGE('',*,*,#6107,.T.);
#8491=ORIENTED_EDGE('',*,*,#6031,.F.);
#8492=ORIENTED_EDGE('',*,*,#6108,.T.);
#8493=ORIENTED_EDGE('',*,*,#6021,.F.);
#8494=ORIENTED_EDGE('',*,*,#6109,.T.);
#8495=ORIENTED_EDGE('',*,*,#6015,.F.);
#8496=ORIENTED_EDGE('',*,*,#6110,.T.);
#8497=ORIENTED_EDGE('',*,*,#6101,.F.);
#8498=ORIENTED_EDGE('',*,*,#6102,.F.);
#8499=ORIENTED_EDGE('',*,*,#6110,.F.);
#8500=ORIENTED_EDGE('',*,*,#6014,.F.);
#8501=ORIENTED_EDGE('',*,*,#6111,.T.);
#8502=ORIENTED_EDGE('',*,*,#6006,.F.);
#8503=ORIENTED_EDGE('',*,*,#6112,.T.);
#8504=ORIENTED_EDGE('',*,*,#5998,.F.);
#8505=ORIENTED_EDGE('',*,*,#6113,.T.);
#8506=ORIENTED_EDGE('',*,*,#6072,.T.);
#8507=ORIENTED_EDGE('',*,*,#6114,.T.);
#8508=ORIENTED_EDGE('',*,*,#6114,.F.);
#8509=ORIENTED_EDGE('',*,*,#6115,.T.);
#8510=ORIENTED_EDGE('',*,*,#6083,.T.);
#8511=ORIENTED_EDGE('',*,*,#6115,.F.);
#8512=ORIENTED_EDGE('',*,*,#6116,.T.);
#8513=ORIENTED_EDGE('',*,*,#6117,.T.);
#8514=ORIENTED_EDGE('',*,*,#6118,.T.);
#8515=ORIENTED_EDGE('',*,*,#6119,.T.);
#8516=ORIENTED_EDGE('',*,*,#6120,.T.);
#8517=ORIENTED_EDGE('',*,*,#6121,.T.);
#8518=ORIENTED_EDGE('',*,*,#6122,.T.);
#8519=ORIENTED_EDGE('',*,*,#6123,.T.);
#8520=ORIENTED_EDGE('',*,*,#6124,.T.);
#8521=ORIENTED_EDGE('',*,*,#6125,.T.);
#8522=ORIENTED_EDGE('',*,*,#6097,.F.);
#8523=ORIENTED_EDGE('',*,*,#6098,.F.);
#8524=ORIENTED_EDGE('',*,*,#6126,.T.);
#8525=ORIENTED_EDGE('',*,*,#6124,.F.);
#8526=ORIENTED_EDGE('',*,*,#6125,.F.);
#8527=ORIENTED_EDGE('',*,*,#6126,.F.);
#8528=ORIENTED_EDGE('',*,*,#6095,.F.);
#8529=ORIENTED_EDGE('',*,*,#6096,.F.);
#8530=ORIENTED_EDGE('',*,*,#6127,.T.);
#8531=ORIENTED_EDGE('',*,*,#6122,.F.);
#8532=ORIENTED_EDGE('',*,*,#6123,.F.);
#8533=ORIENTED_EDGE('',*,*,#6127,.F.);
#8534=ORIENTED_EDGE('',*,*,#6093,.F.);
#8535=ORIENTED_EDGE('',*,*,#6094,.F.);
#8536=ORIENTED_EDGE('',*,*,#6128,.T.);
#8537=ORIENTED_EDGE('',*,*,#6120,.F.);
#8538=ORIENTED_EDGE('',*,*,#6121,.F.);
#8539=ORIENTED_EDGE('',*,*,#6128,.F.);
#8540=ORIENTED_EDGE('',*,*,#6091,.F.);
#8541=ORIENTED_EDGE('',*,*,#6092,.F.);
#8542=ORIENTED_EDGE('',*,*,#6129,.T.);
#8543=ORIENTED_EDGE('',*,*,#6118,.F.);
#8544=ORIENTED_EDGE('',*,*,#6119,.F.);
#8545=ORIENTED_EDGE('',*,*,#6129,.F.);
#8546=ORIENTED_EDGE('',*,*,#6089,.F.);
#8547=ORIENTED_EDGE('',*,*,#6090,.F.);
#8548=ORIENTED_EDGE('',*,*,#6130,.T.);
#8549=ORIENTED_EDGE('',*,*,#6116,.F.);
#8550=ORIENTED_EDGE('',*,*,#6117,.F.);
#8551=ORIENTED_EDGE('',*,*,#6130,.F.);
#8552=ORIENTED_EDGE('',*,*,#6131,.T.);
#8553=ORIENTED_EDGE('',*,*,#6132,.T.);
#8554=ORIENTED_EDGE('',*,*,#6068,.T.);
#8555=ORIENTED_EDGE('',*,*,#6132,.F.);
#8556=ORIENTED_EDGE('',*,*,#6071,.F.);
#8557=ORIENTED_EDGE('',*,*,#6133,.T.);
#8558=ORIENTED_EDGE('',*,*,#6131,.F.);
#8559=ORIENTED_EDGE('',*,*,#6133,.F.);
#8560=ORIENTED_EDGE('',*,*,#6134,.T.);
#8561=ORIENTED_EDGE('',*,*,#6069,.F.);
#8562=ORIENTED_EDGE('',*,*,#6134,.F.);
#8563=ORIENTED_EDGE('',*,*,#6135,.T.);
#8564=ORIENTED_EDGE('',*,*,#6136,.T.);
#8565=ORIENTED_EDGE('',*,*,#6135,.F.);
#8566=ORIENTED_EDGE('',*,*,#6136,.F.);
#8567=ORIENTED_EDGE('',*,*,#6074,.T.);
#8568=ORIENTED_EDGE('',*,*,#6137,.T.);
#8569=ORIENTED_EDGE('',*,*,#6138,.T.);
#8570=ORIENTED_EDGE('',*,*,#6139,.T.);
#8571=ORIENTED_EDGE('',*,*,#6140,.T.);
#8572=ORIENTED_EDGE('',*,*,#6141,.T.);
#8573=ORIENTED_EDGE('',*,*,#6142,.T.);
#8574=ORIENTED_EDGE('',*,*,#6143,.T.);
#8575=ORIENTED_EDGE('',*,*,#6144,.T.);
#8576=ORIENTED_EDGE('',*,*,#6145,.T.);
#8577=ORIENTED_EDGE('',*,*,#6146,.T.);
#8578=ORIENTED_EDGE('',*,*,#6147,.T.);
#8579=ORIENTED_EDGE('',*,*,#6148,.T.);
#8580=ORIENTED_EDGE('',*,*,#6149,.T.);
#8581=ORIENTED_EDGE('',*,*,#6150,.T.);
#8582=ORIENTED_EDGE('',*,*,#6151,.T.);
#8583=ORIENTED_EDGE('',*,*,#6152,.T.);
#8584=ORIENTED_EDGE('',*,*,#6153,.T.);
#8585=ORIENTED_EDGE('',*,*,#6154,.T.);
#8586=ORIENTED_EDGE('',*,*,#6155,.T.);
#8587=ORIENTED_EDGE('',*,*,#6156,.T.);
#8588=ORIENTED_EDGE('',*,*,#6157,.T.);
#8589=ORIENTED_EDGE('',*,*,#6158,.T.);
#8590=ORIENTED_EDGE('',*,*,#6159,.T.);
#8591=ORIENTED_EDGE('',*,*,#6160,.T.);
#8592=ORIENTED_EDGE('',*,*,#6161,.T.);
#8593=ORIENTED_EDGE('',*,*,#6162,.T.);
#8594=ORIENTED_EDGE('',*,*,#6163,.T.);
#8595=ORIENTED_EDGE('',*,*,#6164,.T.);
#8596=ORIENTED_EDGE('',*,*,#6165,.T.);
#8597=ORIENTED_EDGE('',*,*,#6166,.T.);
#8598=ORIENTED_EDGE('',*,*,#6167,.T.);
#8599=ORIENTED_EDGE('',*,*,#6168,.T.);
#8600=ORIENTED_EDGE('',*,*,#6169,.T.);
#8601=ORIENTED_EDGE('',*,*,#6170,.T.);
#8602=ORIENTED_EDGE('',*,*,#6171,.T.);
#8603=ORIENTED_EDGE('',*,*,#6172,.T.);
#8604=ORIENTED_EDGE('',*,*,#6173,.T.);
#8605=ORIENTED_EDGE('',*,*,#6174,.T.);
#8606=ORIENTED_EDGE('',*,*,#6175,.T.);
#8607=ORIENTED_EDGE('',*,*,#6176,.T.);
#8608=ORIENTED_EDGE('',*,*,#6112,.F.);
#8609=ORIENTED_EDGE('',*,*,#6005,.F.);
#8610=ORIENTED_EDGE('',*,*,#6177,.F.);
#8611=ORIENTED_EDGE('',*,*,#6172,.F.);
#8612=ORIENTED_EDGE('',*,*,#6178,.F.);
#8613=ORIENTED_EDGE('',*,*,#5999,.F.);
#8614=ORIENTED_EDGE('',*,*,#6177,.T.);
#8615=ORIENTED_EDGE('',*,*,#6004,.F.);
#8616=ORIENTED_EDGE('',*,*,#6179,.F.);
#8617=ORIENTED_EDGE('',*,*,#6169,.F.);
#8618=ORIENTED_EDGE('',*,*,#6178,.T.);
#8619=ORIENTED_EDGE('',*,*,#6171,.F.);
#8620=ORIENTED_EDGE('',*,*,#6180,.F.);
#8621=ORIENTED_EDGE('',*,*,#5992,.F.);
#8622=ORIENTED_EDGE('',*,*,#6003,.F.);
#8623=ORIENTED_EDGE('',*,*,#6057,.F.);
#8624=ORIENTED_EDGE('',*,*,#5993,.F.);
#8625=ORIENTED_EDGE('',*,*,#6180,.T.);
#8626=ORIENTED_EDGE('',*,*,#6170,.F.);
#8627=ORIENTED_EDGE('',*,*,#6179,.T.);
#8628=ORIENTED_EDGE('',*,*,#6111,.F.);
#8629=ORIENTED_EDGE('',*,*,#6013,.F.);
#8630=ORIENTED_EDGE('',*,*,#6181,.F.);
#8631=ORIENTED_EDGE('',*,*,#6168,.F.);
#8632=ORIENTED_EDGE('',*,*,#6182,.F.);
#8633=ORIENTED_EDGE('',*,*,#6007,.F.);
#8634=ORIENTED_EDGE('',*,*,#6181,.T.);
#8635=ORIENTED_EDGE('',*,*,#6012,.F.);
#8636=ORIENTED_EDGE('',*,*,#6183,.F.);
#8637=ORIENTED_EDGE('',*,*,#6165,.F.);
#8638=ORIENTED_EDGE('',*,*,#6182,.T.);
#8639=ORIENTED_EDGE('',*,*,#6167,.F.);
#8640=ORIENTED_EDGE('',*,*,#6184,.F.);
#8641=ORIENTED_EDGE('',*,*,#6000,.F.);
#8642=ORIENTED_EDGE('',*,*,#6011,.F.);
#8643=ORIENTED_EDGE('',*,*,#6058,.F.);
#8644=ORIENTED_EDGE('',*,*,#6001,.F.);
#8645=ORIENTED_EDGE('',*,*,#6184,.T.);
#8646=ORIENTED_EDGE('',*,*,#6166,.F.);
#8647=ORIENTED_EDGE('',*,*,#6183,.T.);
#8648=ORIENTED_EDGE('',*,*,#6109,.F.);
#8649=ORIENTED_EDGE('',*,*,#6020,.F.);
#8650=ORIENTED_EDGE('',*,*,#6185,.F.);
#8651=ORIENTED_EDGE('',*,*,#6164,.F.);
#8652=ORIENTED_EDGE('',*,*,#6186,.F.);
#8653=ORIENTED_EDGE('',*,*,#6016,.F.);
#8654=ORIENTED_EDGE('',*,*,#6185,.T.);
#8655=ORIENTED_EDGE('',*,*,#6019,.F.);
#8656=ORIENTED_EDGE('',*,*,#6187,.F.);
#8657=ORIENTED_EDGE('',*,*,#6161,.F.);
#8658=ORIENTED_EDGE('',*,*,#6186,.T.);
#8659=ORIENTED_EDGE('',*,*,#6163,.F.);
#8660=ORIENTED_EDGE('',*,*,#6188,.F.);
#8661=ORIENTED_EDGE('',*,*,#6008,.F.);
#8662=ORIENTED_EDGE('',*,*,#6018,.F.);
#8663=ORIENTED_EDGE('',*,*,#6059,.F.);
#8664=ORIENTED_EDGE('',*,*,#6009,.F.);
#8665=ORIENTED_EDGE('',*,*,#6188,.T.);
#8666=ORIENTED_EDGE('',*,*,#6162,.F.);
#8667=ORIENTED_EDGE('',*,*,#6187,.T.);
#8668=ORIENTED_EDGE('',*,*,#6108,.F.);
#8669=ORIENTED_EDGE('',*,*,#6030,.F.);
#8670=ORIENTED_EDGE('',*,*,#6189,.F.);
#8671=ORIENTED_EDGE('',*,*,#6157,.F.);
#8672=ORIENTED_EDGE('',*,*,#6190,.F.);
#8673=ORIENTED_EDGE('',*,*,#6022,.F.);
#8674=ORIENTED_EDGE('',*,*,#6189,.T.);
#8675=ORIENTED_EDGE('',*,*,#6029,.F.);
#8676=ORIENTED_EDGE('',*,*,#6191,.F.);
#8677=ORIENTED_EDGE('',*,*,#6158,.F.);
#8678=ORIENTED_EDGE('',*,*,#6190,.T.);
#8679=ORIENTED_EDGE('',*,*,#6160,.F.);
#8680=ORIENTED_EDGE('',*,*,#6192,.F.);
#8681=ORIENTED_EDGE('',*,*,#6023,.F.);
#8682=ORIENTED_EDGE('',*,*,#6028,.F.);
#8683=ORIENTED_EDGE('',*,*,#6060,.F.);
#8684=ORIENTED_EDGE('',*,*,#6024,.F.);
#8685=ORIENTED_EDGE('',*,*,#6192,.T.);
#8686=ORIENTED_EDGE('',*,*,#6159,.F.);
#8687=ORIENTED_EDGE('',*,*,#6191,.T.);
#8688=ORIENTED_EDGE('',*,*,#6107,.F.);
#8689=ORIENTED_EDGE('',*,*,#6038,.F.);
#8690=ORIENTED_EDGE('',*,*,#6193,.F.);
#8691=ORIENTED_EDGE('',*,*,#6156,.F.);
#8692=ORIENTED_EDGE('',*,*,#6194,.F.);
#8693=ORIENTED_EDGE('',*,*,#6032,.F.);
#8694=ORIENTED_EDGE('',*,*,#6193,.T.);
#8695=ORIENTED_EDGE('',*,*,#6037,.F.);
#8696=ORIENTED_EDGE('',*,*,#6195,.F.);
#8697=ORIENTED_EDGE('',*,*,#6153,.F.);
#8698=ORIENTED_EDGE('',*,*,#6194,.T.);
#8699=ORIENTED_EDGE('',*,*,#6155,.F.);
#8700=ORIENTED_EDGE('',*,*,#6196,.F.);
#8701=ORIENTED_EDGE('',*,*,#6025,.F.);
#8702=ORIENTED_EDGE('',*,*,#6036,.F.);
#8703=ORIENTED_EDGE('',*,*,#6061,.F.);
#8704=ORIENTED_EDGE('',*,*,#6026,.F.);
#8705=ORIENTED_EDGE('',*,*,#6196,.T.);
#8706=ORIENTED_EDGE('',*,*,#6154,.F.);
#8707=ORIENTED_EDGE('',*,*,#6195,.T.);
#8708=ORIENTED_EDGE('',*,*,#6106,.F.);
#8709=ORIENTED_EDGE('',*,*,#6046,.F.);
#8710=ORIENTED_EDGE('',*,*,#6197,.F.);
#8711=ORIENTED_EDGE('',*,*,#6152,.F.);
#8712=ORIENTED_EDGE('',*,*,#6198,.F.);
#8713=ORIENTED_EDGE('',*,*,#6040,.F.);
#8714=ORIENTED_EDGE('',*,*,#6197,.T.);
#8715=ORIENTED_EDGE('',*,*,#6045,.F.);
#8716=ORIENTED_EDGE('',*,*,#6199,.F.);
#8717=ORIENTED_EDGE('',*,*,#6149,.F.);
#8718=ORIENTED_EDGE('',*,*,#6198,.T.);
#8719=ORIENTED_EDGE('',*,*,#6151,.F.);
#8720=ORIENTED_EDGE('',*,*,#6200,.F.);
#8721=ORIENTED_EDGE('',*,*,#6033,.F.);
#8722=ORIENTED_EDGE('',*,*,#6044,.F.);
#8723=ORIENTED_EDGE('',*,*,#6062,.F.);
#8724=ORIENTED_EDGE('',*,*,#6034,.F.);
#8725=ORIENTED_EDGE('',*,*,#6200,.T.);
#8726=ORIENTED_EDGE('',*,*,#6150,.F.);
#8727=ORIENTED_EDGE('',*,*,#6199,.T.);
#8728=ORIENTED_EDGE('',*,*,#6105,.F.);
#8729=ORIENTED_EDGE('',*,*,#6054,.F.);
#8730=ORIENTED_EDGE('',*,*,#6201,.F.);
#8731=ORIENTED_EDGE('',*,*,#6148,.F.);
#8732=ORIENTED_EDGE('',*,*,#6202,.F.);
#8733=ORIENTED_EDGE('',*,*,#6048,.F.);
#8734=ORIENTED_EDGE('',*,*,#6201,.T.);
#8735=ORIENTED_EDGE('',*,*,#6053,.F.);
#8736=ORIENTED_EDGE('',*,*,#6203,.F.);
#8737=ORIENTED_EDGE('',*,*,#6145,.F.);
#8738=ORIENTED_EDGE('',*,*,#6202,.T.);
#8739=ORIENTED_EDGE('',*,*,#6147,.F.);
#8740=ORIENTED_EDGE('',*,*,#6204,.F.);
#8741=ORIENTED_EDGE('',*,*,#6041,.F.);
#8742=ORIENTED_EDGE('',*,*,#6052,.F.);
#8743=ORIENTED_EDGE('',*,*,#6063,.F.);
#8744=ORIENTED_EDGE('',*,*,#6042,.F.);
#8745=ORIENTED_EDGE('',*,*,#6204,.T.);
#8746=ORIENTED_EDGE('',*,*,#6146,.F.);
#8747=ORIENTED_EDGE('',*,*,#6203,.T.);
#8748=ORIENTED_EDGE('',*,*,#6104,.F.);
#8749=ORIENTED_EDGE('',*,*,#6079,.F.);
#8750=ORIENTED_EDGE('',*,*,#6205,.F.);
#8751=ORIENTED_EDGE('',*,*,#6144,.F.);
#8752=ORIENTED_EDGE('',*,*,#6206,.F.);
#8753=ORIENTED_EDGE('',*,*,#6056,.F.);
#8754=ORIENTED_EDGE('',*,*,#6205,.T.);
#8755=ORIENTED_EDGE('',*,*,#6078,.F.);
#8756=ORIENTED_EDGE('',*,*,#6207,.F.);
#8757=ORIENTED_EDGE('',*,*,#6141,.F.);
#8758=ORIENTED_EDGE('',*,*,#6206,.T.);
#8759=ORIENTED_EDGE('',*,*,#6143,.F.);
#8760=ORIENTED_EDGE('',*,*,#6208,.F.);
#8761=ORIENTED_EDGE('',*,*,#6049,.F.);
#8762=ORIENTED_EDGE('',*,*,#6077,.F.);
#8763=ORIENTED_EDGE('',*,*,#6064,.F.);
#8764=ORIENTED_EDGE('',*,*,#6050,.F.);
#8765=ORIENTED_EDGE('',*,*,#6208,.T.);
#8766=ORIENTED_EDGE('',*,*,#6142,.F.);
#8767=ORIENTED_EDGE('',*,*,#6207,.T.);
#8768=ORIENTED_EDGE('',*,*,#6103,.F.);
#8769=ORIENTED_EDGE('',*,*,#5987,.F.);
#8770=ORIENTED_EDGE('',*,*,#6209,.F.);
#8771=ORIENTED_EDGE('',*,*,#6140,.F.);
#8772=ORIENTED_EDGE('',*,*,#6210,.F.);
#8773=ORIENTED_EDGE('',*,*,#6081,.F.);
#8774=ORIENTED_EDGE('',*,*,#6209,.T.);
#8775=ORIENTED_EDGE('',*,*,#5986,.F.);
#8776=ORIENTED_EDGE('',*,*,#6211,.F.);
#8777=ORIENTED_EDGE('',*,*,#6137,.F.);
#8778=ORIENTED_EDGE('',*,*,#6210,.T.);
#8779=ORIENTED_EDGE('',*,*,#6139,.F.);
#8780=ORIENTED_EDGE('',*,*,#6212,.F.);
#8781=ORIENTED_EDGE('',*,*,#6075,.F.);
#8782=ORIENTED_EDGE('',*,*,#5985,.F.);
#8783=ORIENTED_EDGE('',*,*,#6066,.F.);
#8784=ORIENTED_EDGE('',*,*,#6076,.F.);
#8785=ORIENTED_EDGE('',*,*,#6212,.T.);
#8786=ORIENTED_EDGE('',*,*,#6138,.F.);
#8787=ORIENTED_EDGE('',*,*,#6211,.T.);
#8788=ORIENTED_EDGE('',*,*,#6113,.F.);
#8789=ORIENTED_EDGE('',*,*,#5997,.F.);
#8790=ORIENTED_EDGE('',*,*,#6213,.F.);
#8791=ORIENTED_EDGE('',*,*,#6176,.F.);
#8792=ORIENTED_EDGE('',*,*,#6214,.F.);
#8793=ORIENTED_EDGE('',*,*,#5989,.F.);
#8794=ORIENTED_EDGE('',*,*,#6213,.T.);
#8795=ORIENTED_EDGE('',*,*,#5996,.F.);
#8796=ORIENTED_EDGE('',*,*,#6215,.F.);
#8797=ORIENTED_EDGE('',*,*,#6173,.F.);
#8798=ORIENTED_EDGE('',*,*,#6214,.T.);
#8799=ORIENTED_EDGE('',*,*,#6175,.F.);
#8800=ORIENTED_EDGE('',*,*,#6216,.F.);
#8801=ORIENTED_EDGE('',*,*,#5990,.F.);
#8802=ORIENTED_EDGE('',*,*,#5995,.F.);
#8803=ORIENTED_EDGE('',*,*,#6067,.F.);
#8804=ORIENTED_EDGE('',*,*,#5991,.F.);
#8805=ORIENTED_EDGE('',*,*,#6216,.T.);
#8806=ORIENTED_EDGE('',*,*,#6174,.F.);
#8807=ORIENTED_EDGE('',*,*,#6215,.T.);
#8808=ORIENTED_EDGE('',*,*,#6217,.F.);
#8809=ORIENTED_EDGE('',*,*,#6218,.F.);
#8810=ORIENTED_EDGE('',*,*,#6219,.T.);
#8811=ORIENTED_EDGE('',*,*,#6220,.F.);
#8812=ORIENTED_EDGE('',*,*,#6221,.F.);
#8813=ORIENTED_EDGE('',*,*,#6222,.F.);
#8814=ORIENTED_EDGE('',*,*,#6223,.F.);
#8815=ORIENTED_EDGE('',*,*,#6224,.F.);
#8816=ORIENTED_EDGE('',*,*,#6225,.F.);
#8817=ORIENTED_EDGE('',*,*,#6226,.F.);
#8818=ORIENTED_EDGE('',*,*,#6227,.F.);
#8819=ORIENTED_EDGE('',*,*,#6228,.F.);
#8820=ORIENTED_EDGE('',*,*,#6229,.F.);
#8821=ORIENTED_EDGE('',*,*,#6230,.F.);
#8822=ORIENTED_EDGE('',*,*,#6231,.F.);
#8823=ORIENTED_EDGE('',*,*,#6232,.F.);
#8824=ORIENTED_EDGE('',*,*,#6233,.F.);
#8825=ORIENTED_EDGE('',*,*,#6234,.F.);
#8826=ORIENTED_EDGE('',*,*,#6235,.F.);
#8827=ORIENTED_EDGE('',*,*,#6236,.F.);
#8828=ORIENTED_EDGE('',*,*,#6237,.F.);
#8829=ORIENTED_EDGE('',*,*,#6238,.F.);
#8830=ORIENTED_EDGE('',*,*,#6239,.F.);
#8831=ORIENTED_EDGE('',*,*,#6240,.F.);
#8832=ORIENTED_EDGE('',*,*,#6241,.F.);
#8833=ORIENTED_EDGE('',*,*,#6242,.F.);
#8834=ORIENTED_EDGE('',*,*,#6243,.F.);
#8835=ORIENTED_EDGE('',*,*,#6244,.F.);
#8836=ORIENTED_EDGE('',*,*,#6245,.T.);
#8837=ORIENTED_EDGE('',*,*,#6230,.T.);
#8838=ORIENTED_EDGE('',*,*,#6246,.F.);
#8839=ORIENTED_EDGE('',*,*,#6247,.F.);
#8840=ORIENTED_EDGE('',*,*,#6248,.T.);
#8841=ORIENTED_EDGE('',*,*,#6234,.T.);
#8842=ORIENTED_EDGE('',*,*,#6249,.F.);
#8843=ORIENTED_EDGE('',*,*,#6250,.F.);
#8844=ORIENTED_EDGE('',*,*,#6251,.T.);
#8845=ORIENTED_EDGE('',*,*,#6238,.T.);
#8846=ORIENTED_EDGE('',*,*,#6252,.F.);
#8847=ORIENTED_EDGE('',*,*,#6221,.T.);
#8848=ORIENTED_EDGE('',*,*,#6253,.T.);
#8849=ORIENTED_EDGE('',*,*,#6254,.F.);
#8850=ORIENTED_EDGE('',*,*,#6255,.T.);
#8851=ORIENTED_EDGE('',*,*,#6256,.F.);
#8852=ORIENTED_EDGE('',*,*,#6257,.T.);
#8853=ORIENTED_EDGE('',*,*,#6222,.T.);
#8854=ORIENTED_EDGE('',*,*,#6255,.F.);
#8855=ORIENTED_EDGE('',*,*,#6258,.F.);
#8856=ORIENTED_EDGE('',*,*,#6259,.T.);
#8857=ORIENTED_EDGE('',*,*,#6226,.T.);
#8858=ORIENTED_EDGE('',*,*,#6260,.F.);
#8859=ORIENTED_EDGE('',*,*,#6261,.T.);
#8860=ORIENTED_EDGE('',*,*,#6262,.T.);
#8861=ORIENTED_EDGE('',*,*,#6263,.T.);
#8862=ORIENTED_EDGE('',*,*,#6218,.T.);
#8863=ORIENTED_EDGE('',*,*,#6263,.F.);
#8864=ORIENTED_EDGE('',*,*,#6264,.T.);
#8865=ORIENTED_EDGE('',*,*,#6265,.T.);
#8866=ORIENTED_EDGE('',*,*,#6266,.T.);
#8867=ORIENTED_EDGE('',*,*,#6267,.T.);
#8868=ORIENTED_EDGE('',*,*,#6266,.F.);
#8869=ORIENTED_EDGE('',*,*,#6268,.T.);
#8870=ORIENTED_EDGE('',*,*,#6269,.T.);
#8871=ORIENTED_EDGE('',*,*,#6270,.T.);
#8872=ORIENTED_EDGE('',*,*,#6250,.T.);
#8873=ORIENTED_EDGE('',*,*,#6271,.T.);
#8874=ORIENTED_EDGE('',*,*,#6272,.T.);
#8875=ORIENTED_EDGE('',*,*,#6273,.T.);
#8876=ORIENTED_EDGE('',*,*,#6247,.T.);
#8877=ORIENTED_EDGE('',*,*,#6274,.T.);
#8878=ORIENTED_EDGE('',*,*,#6275,.T.);
#8879=ORIENTED_EDGE('',*,*,#6276,.T.);
#8880=ORIENTED_EDGE('',*,*,#6244,.T.);
#8881=ORIENTED_EDGE('',*,*,#6277,.T.);
#8882=ORIENTED_EDGE('',*,*,#6278,.T.);
#8883=ORIENTED_EDGE('',*,*,#6279,.T.);
#8884=ORIENTED_EDGE('',*,*,#6258,.T.);
#8885=ORIENTED_EDGE('',*,*,#6280,.T.);
#8886=ORIENTED_EDGE('',*,*,#6281,.T.);
#8887=ORIENTED_EDGE('',*,*,#6282,.T.);
#8888=ORIENTED_EDGE('',*,*,#6256,.T.);
#8889=ORIENTED_EDGE('',*,*,#6254,.T.);
#8890=ORIENTED_EDGE('',*,*,#6283,.T.);
#8891=ORIENTED_EDGE('',*,*,#6284,.T.);
#8892=ORIENTED_EDGE('',*,*,#6285,.T.);
#8893=ORIENTED_EDGE('',*,*,#6286,.T.);
#8894=ORIENTED_EDGE('',*,*,#6233,.T.);
#8895=ORIENTED_EDGE('',*,*,#6287,.T.);
#8896=ORIENTED_EDGE('',*,*,#6274,.F.);
#8897=ORIENTED_EDGE('',*,*,#6249,.T.);
#8898=ORIENTED_EDGE('',*,*,#6237,.T.);
#8899=ORIENTED_EDGE('',*,*,#6288,.T.);
#8900=ORIENTED_EDGE('',*,*,#6271,.F.);
#8901=ORIENTED_EDGE('',*,*,#6252,.T.);
#8902=ORIENTED_EDGE('',*,*,#6241,.T.);
#8903=ORIENTED_EDGE('',*,*,#6289,.T.);
#8904=ORIENTED_EDGE('',*,*,#6268,.F.);
#8905=ORIENTED_EDGE('',*,*,#6290,.T.);
#8906=ORIENTED_EDGE('',*,*,#6285,.F.);
#8907=ORIENTED_EDGE('',*,*,#6291,.T.);
#8908=ORIENTED_EDGE('',*,*,#6242,.T.);
#8909=ORIENTED_EDGE('',*,*,#6290,.F.);
#8910=ORIENTED_EDGE('',*,*,#6225,.T.);
#8911=ORIENTED_EDGE('',*,*,#6292,.T.);
#8912=ORIENTED_EDGE('',*,*,#6280,.F.);
#8913=ORIENTED_EDGE('',*,*,#6260,.T.);
#8914=ORIENTED_EDGE('',*,*,#6229,.T.);
#8915=ORIENTED_EDGE('',*,*,#6293,.T.);
#8916=ORIENTED_EDGE('',*,*,#6277,.F.);
#8917=ORIENTED_EDGE('',*,*,#6246,.T.);
#8918=ORIENTED_EDGE('',*,*,#6228,.T.);
#8919=ORIENTED_EDGE('',*,*,#6294,.F.);
#8920=ORIENTED_EDGE('',*,*,#6278,.F.);
#8921=ORIENTED_EDGE('',*,*,#6293,.F.);
#8922=ORIENTED_EDGE('',*,*,#6279,.F.);
#8923=ORIENTED_EDGE('',*,*,#6294,.T.);
#8924=ORIENTED_EDGE('',*,*,#6227,.T.);
#8925=ORIENTED_EDGE('',*,*,#6259,.F.);
#8926=ORIENTED_EDGE('',*,*,#6224,.T.);
#8927=ORIENTED_EDGE('',*,*,#6295,.F.);
#8928=ORIENTED_EDGE('',*,*,#6281,.F.);
#8929=ORIENTED_EDGE('',*,*,#6292,.F.);
#8930=ORIENTED_EDGE('',*,*,#6282,.F.);
#8931=ORIENTED_EDGE('',*,*,#6295,.T.);
#8932=ORIENTED_EDGE('',*,*,#6223,.T.);
#8933=ORIENTED_EDGE('',*,*,#6257,.F.);
#8934=ORIENTED_EDGE('',*,*,#6284,.F.);
#8935=ORIENTED_EDGE('',*,*,#6296,.T.);
#8936=ORIENTED_EDGE('',*,*,#6243,.T.);
#8937=ORIENTED_EDGE('',*,*,#6291,.F.);
#8938=ORIENTED_EDGE('',*,*,#6220,.T.);
#8939=ORIENTED_EDGE('',*,*,#6296,.F.);
#8940=ORIENTED_EDGE('',*,*,#6283,.F.);
#8941=ORIENTED_EDGE('',*,*,#6253,.F.);
#8942=ORIENTED_EDGE('',*,*,#6240,.T.);
#8943=ORIENTED_EDGE('',*,*,#6297,.F.);
#8944=ORIENTED_EDGE('',*,*,#6269,.F.);
#8945=ORIENTED_EDGE('',*,*,#6289,.F.);
#8946=ORIENTED_EDGE('',*,*,#6270,.F.);
#8947=ORIENTED_EDGE('',*,*,#6297,.T.);
#8948=ORIENTED_EDGE('',*,*,#6239,.T.);
#8949=ORIENTED_EDGE('',*,*,#6251,.F.);
#8950=ORIENTED_EDGE('',*,*,#6236,.T.);
#8951=ORIENTED_EDGE('',*,*,#6298,.F.);
#8952=ORIENTED_EDGE('',*,*,#6272,.F.);
#8953=ORIENTED_EDGE('',*,*,#6288,.F.);
#8954=ORIENTED_EDGE('',*,*,#6273,.F.);
#8955=ORIENTED_EDGE('',*,*,#6298,.T.);
#8956=ORIENTED_EDGE('',*,*,#6235,.T.);
#8957=ORIENTED_EDGE('',*,*,#6248,.F.);
#8958=ORIENTED_EDGE('',*,*,#6232,.T.);
#8959=ORIENTED_EDGE('',*,*,#6299,.F.);
#8960=ORIENTED_EDGE('',*,*,#6275,.F.);
#8961=ORIENTED_EDGE('',*,*,#6287,.F.);
#8962=ORIENTED_EDGE('',*,*,#6276,.F.);
#8963=ORIENTED_EDGE('',*,*,#6299,.T.);
#8964=ORIENTED_EDGE('',*,*,#6231,.T.);
#8965=ORIENTED_EDGE('',*,*,#6245,.F.);
#8966=ORIENTED_EDGE('',*,*,#6261,.F.);
#8967=ORIENTED_EDGE('',*,*,#6262,.F.);
#8968=ORIENTED_EDGE('',*,*,#6300,.T.);
#8969=ORIENTED_EDGE('',*,*,#6286,.F.);
#8970=ORIENTED_EDGE('',*,*,#6300,.F.);
#8971=ORIENTED_EDGE('',*,*,#6264,.F.);
#8972=ORIENTED_EDGE('',*,*,#6265,.F.);
#8973=ORIENTED_EDGE('',*,*,#6301,.T.);
#8974=ORIENTED_EDGE('',*,*,#6219,.F.);
#8975=ORIENTED_EDGE('',*,*,#6301,.F.);
#8976=ORIENTED_EDGE('',*,*,#6267,.F.);
#8977=ORIENTED_EDGE('',*,*,#6302,.T.);
#8978=ORIENTED_EDGE('',*,*,#6217,.T.);
#8979=ORIENTED_EDGE('',*,*,#6302,.F.);
#8980=ORIENTED_EDGE('',*,*,#6303,.T.);
#8981=ORIENTED_EDGE('',*,*,#6304,.F.);
#8982=ORIENTED_EDGE('',*,*,#6305,.F.);
#8983=ORIENTED_EDGE('',*,*,#6306,.F.);
#8984=ORIENTED_EDGE('',*,*,#6307,.T.);
#8985=ORIENTED_EDGE('',*,*,#6307,.F.);
#8986=ORIENTED_EDGE('',*,*,#6308,.F.);
#8987=ORIENTED_EDGE('',*,*,#6309,.T.);
#8988=ORIENTED_EDGE('',*,*,#6310,.T.);
#8989=ORIENTED_EDGE('',*,*,#6311,.T.);
#8990=ORIENTED_EDGE('',*,*,#6309,.F.);
#8991=ORIENTED_EDGE('',*,*,#6312,.F.);
#8992=ORIENTED_EDGE('',*,*,#6313,.T.);
#8993=ORIENTED_EDGE('',*,*,#6314,.T.);
#8994=ORIENTED_EDGE('',*,*,#6310,.F.);
#8995=ORIENTED_EDGE('',*,*,#6313,.F.);
#8996=ORIENTED_EDGE('',*,*,#6315,.F.);
#8997=ORIENTED_EDGE('',*,*,#6305,.T.);
#8998=ORIENTED_EDGE('',*,*,#6304,.T.);
#8999=ORIENTED_EDGE('',*,*,#6316,.T.);
#9000=ORIENTED_EDGE('',*,*,#6316,.F.);
#9001=ORIENTED_EDGE('',*,*,#6303,.F.);
#9002=ORIENTED_EDGE('',*,*,#6311,.F.);
#9003=ORIENTED_EDGE('',*,*,#6314,.F.);
#9004=ORIENTED_EDGE('',*,*,#6315,.T.);
#9005=ORIENTED_EDGE('',*,*,#6312,.T.);
#9006=ORIENTED_EDGE('',*,*,#6308,.T.);
#9007=ORIENTED_EDGE('',*,*,#6306,.T.);
#9008=ORIENTED_EDGE('',*,*,#6317,.T.);
#9009=ORIENTED_EDGE('',*,*,#6318,.F.);
#9010=ORIENTED_EDGE('',*,*,#6317,.F.);
#9011=ORIENTED_EDGE('',*,*,#6319,.T.);
#9012=ORIENTED_EDGE('',*,*,#6320,.T.);
#9013=ORIENTED_EDGE('',*,*,#6319,.F.);
#9014=ORIENTED_EDGE('',*,*,#6320,.F.);
#9015=ORIENTED_EDGE('',*,*,#6321,.T.);
#9016=ORIENTED_EDGE('',*,*,#6322,.T.);
#9017=ORIENTED_EDGE('',*,*,#6321,.F.);
#9018=ORIENTED_EDGE('',*,*,#6322,.F.);
#9019=ORIENTED_EDGE('',*,*,#6323,.T.);
#9020=ORIENTED_EDGE('',*,*,#6324,.T.);
#9021=ORIENTED_EDGE('',*,*,#6323,.F.);
#9022=ORIENTED_EDGE('',*,*,#6324,.F.);
#9023=ORIENTED_EDGE('',*,*,#6325,.T.);
#9024=ORIENTED_EDGE('',*,*,#6325,.F.);
#9025=ORIENTED_EDGE('',*,*,#6326,.T.);
#9026=ORIENTED_EDGE('',*,*,#6327,.T.);
#9027=ORIENTED_EDGE('',*,*,#6326,.F.);
#9028=ORIENTED_EDGE('',*,*,#6328,.T.);
#9029=ORIENTED_EDGE('',*,*,#6327,.F.);
#9030=ORIENTED_EDGE('',*,*,#6328,.F.);
#9031=ORIENTED_EDGE('',*,*,#6329,.T.);
#9032=ORIENTED_EDGE('',*,*,#6330,.T.);
#9033=ORIENTED_EDGE('',*,*,#6331,.T.);
#9034=ORIENTED_EDGE('',*,*,#6329,.F.);
#9035=ORIENTED_EDGE('',*,*,#6332,.T.);
#9036=ORIENTED_EDGE('',*,*,#6333,.T.);
#9037=ORIENTED_EDGE('',*,*,#6334,.T.);
#9038=ORIENTED_EDGE('',*,*,#6330,.F.);
#9039=ORIENTED_EDGE('',*,*,#6331,.F.);
#9040=ORIENTED_EDGE('',*,*,#6334,.F.);
#9041=ORIENTED_EDGE('',*,*,#6332,.F.);
#9042=ORIENTED_EDGE('',*,*,#6333,.F.);
#9043=ORIENTED_EDGE('',*,*,#6335,.T.);
#9044=ORIENTED_EDGE('',*,*,#6336,.T.);
#9045=ORIENTED_EDGE('',*,*,#6337,.T.);
#9046=ORIENTED_EDGE('',*,*,#6335,.F.);
#9047=ORIENTED_EDGE('',*,*,#6338,.T.);
#9048=ORIENTED_EDGE('',*,*,#6339,.T.);
#9049=ORIENTED_EDGE('',*,*,#6340,.T.);
#9050=ORIENTED_EDGE('',*,*,#6336,.F.);
#9051=ORIENTED_EDGE('',*,*,#6337,.F.);
#9052=ORIENTED_EDGE('',*,*,#6340,.F.);
#9053=ORIENTED_EDGE('',*,*,#6338,.F.);
#9054=ORIENTED_EDGE('',*,*,#6339,.F.);
#9055=ORIENTED_EDGE('',*,*,#6341,.T.);
#9056=ORIENTED_EDGE('',*,*,#6342,.T.);
#9057=ORIENTED_EDGE('',*,*,#6341,.F.);
#9058=ORIENTED_EDGE('',*,*,#6343,.T.);
#9059=ORIENTED_EDGE('',*,*,#6342,.F.);
#9060=ORIENTED_EDGE('',*,*,#6343,.F.);
#9061=ORIENTED_EDGE('',*,*,#6344,.T.);
#9062=ORIENTED_EDGE('',*,*,#6318,.T.);
#9063=ORIENTED_EDGE('',*,*,#6344,.F.);
#9064=ORIENTED_EDGE('',*,*,#6345,.T.);
#9065=ORIENTED_EDGE('',*,*,#6345,.F.);
#9066=ORIENTED_EDGE('',*,*,#6346,.F.);
#9067=ORIENTED_EDGE('',*,*,#6347,.F.);
#9068=ORIENTED_EDGE('',*,*,#6348,.T.);
#9069=ORIENTED_EDGE('',*,*,#6346,.T.);
#9070=ORIENTED_EDGE('',*,*,#6348,.F.);
#9071=ORIENTED_EDGE('',*,*,#6349,.T.);
#9072=ORIENTED_EDGE('',*,*,#6350,.T.);
#9073=ORIENTED_EDGE('',*,*,#6351,.T.);
#9074=ORIENTED_EDGE('',*,*,#6347,.T.);
#9075=ORIENTED_EDGE('',*,*,#6351,.F.);
#9076=ORIENTED_EDGE('',*,*,#6352,.T.);
#9077=ORIENTED_EDGE('',*,*,#6353,.F.);
#9078=ORIENTED_EDGE('',*,*,#6354,.T.);
#9079=ORIENTED_EDGE('',*,*,#6355,.T.);
#9080=ORIENTED_EDGE('',*,*,#6356,.T.);
#9081=ORIENTED_EDGE('',*,*,#6353,.T.);
#9082=ORIENTED_EDGE('',*,*,#6356,.F.);
#9083=ORIENTED_EDGE('',*,*,#6349,.F.);
#9084=ORIENTED_EDGE('',*,*,#6350,.F.);
#9085=ORIENTED_EDGE('',*,*,#6357,.T.);
#9086=ORIENTED_EDGE('',*,*,#6352,.F.);
#9087=ORIENTED_EDGE('',*,*,#6357,.F.);
#9088=ORIENTED_EDGE('',*,*,#6354,.F.);
#9089=ORIENTED_EDGE('',*,*,#6355,.F.);
#9090=ORIENTED_EDGE('',*,*,#6358,.T.);
#9091=ORIENTED_EDGE('',*,*,#6359,.T.);
#9092=ORIENTED_EDGE('',*,*,#6358,.F.);
#9093=ORIENTED_EDGE('',*,*,#6360,.T.);
#9094=ORIENTED_EDGE('',*,*,#6360,.F.);
#9095=ORIENTED_EDGE('',*,*,#6361,.T.);
#9096=ORIENTED_EDGE('',*,*,#6362,.T.);
#9097=ORIENTED_EDGE('',*,*,#6361,.F.);
#9098=ORIENTED_EDGE('',*,*,#6362,.F.);
#9099=ORIENTED_EDGE('',*,*,#6363,.T.);
#9100=ORIENTED_EDGE('',*,*,#6364,.F.);
#9101=ORIENTED_EDGE('',*,*,#6363,.F.);
#9102=ORIENTED_EDGE('',*,*,#6359,.F.);
#9103=ORIENTED_EDGE('',*,*,#6364,.T.);
#9104=ORIENTED_EDGE('',*,*,#6365,.F.);
#9105=ORIENTED_EDGE('',*,*,#6366,.T.);
#9106=ORIENTED_EDGE('',*,*,#6365,.T.);
#9107=ORIENTED_EDGE('',*,*,#6366,.F.);
#9108=ORIENTED_EDGE('',*,*,#6367,.F.);
#9109=ORIENTED_EDGE('',*,*,#6368,.T.);
#9110=ORIENTED_EDGE('',*,*,#6369,.F.);
#9111=ORIENTED_EDGE('',*,*,#6370,.T.);
#9112=ORIENTED_EDGE('',*,*,#6371,.F.);
#9113=ORIENTED_EDGE('',*,*,#6372,.T.);
#9114=ORIENTED_EDGE('',*,*,#6373,.F.);
#9115=ORIENTED_EDGE('',*,*,#6374,.T.);
#9116=ORIENTED_EDGE('',*,*,#6375,.F.);
#9117=ORIENTED_EDGE('',*,*,#6376,.T.);
#9118=ORIENTED_EDGE('',*,*,#6377,.F.);
#9119=ORIENTED_EDGE('',*,*,#6378,.T.);
#9120=ORIENTED_EDGE('',*,*,#6379,.F.);
#9121=ORIENTED_EDGE('',*,*,#6380,.F.);
#9122=ORIENTED_EDGE('',*,*,#6381,.T.);
#9123=ORIENTED_EDGE('',*,*,#6382,.F.);
#9124=ORIENTED_EDGE('',*,*,#6383,.T.);
#9125=ORIENTED_EDGE('',*,*,#6384,.F.);
#9126=ORIENTED_EDGE('',*,*,#6385,.T.);
#9127=ORIENTED_EDGE('',*,*,#6386,.F.);
#9128=ORIENTED_EDGE('',*,*,#6387,.T.);
#9129=ORIENTED_EDGE('',*,*,#6388,.F.);
#9130=ORIENTED_EDGE('',*,*,#6389,.T.);
#9131=ORIENTED_EDGE('',*,*,#6390,.F.);
#9132=ORIENTED_EDGE('',*,*,#6391,.T.);
#9133=ORIENTED_EDGE('',*,*,#6392,.F.);
#9134=ORIENTED_EDGE('',*,*,#6393,.T.);
#9135=ORIENTED_EDGE('',*,*,#6394,.T.);
#9136=ORIENTED_EDGE('',*,*,#6375,.T.);
#9137=ORIENTED_EDGE('',*,*,#6395,.T.);
#9138=ORIENTED_EDGE('',*,*,#6396,.F.);
#9139=ORIENTED_EDGE('',*,*,#6397,.T.);
#9140=ORIENTED_EDGE('',*,*,#6385,.F.);
#9141=ORIENTED_EDGE('',*,*,#6398,.T.);
#9142=ORIENTED_EDGE('',*,*,#6396,.T.);
#9143=ORIENTED_EDGE('',*,*,#6399,.T.);
#9144=ORIENTED_EDGE('',*,*,#6373,.T.);
#9145=ORIENTED_EDGE('',*,*,#6400,.T.);
#9146=ORIENTED_EDGE('',*,*,#6401,.F.);
#9147=ORIENTED_EDGE('',*,*,#6402,.T.);
#9148=ORIENTED_EDGE('',*,*,#6387,.F.);
#9149=ORIENTED_EDGE('',*,*,#6403,.T.);
#9150=ORIENTED_EDGE('',*,*,#6401,.T.);
#9151=ORIENTED_EDGE('',*,*,#6404,.T.);
#9152=ORIENTED_EDGE('',*,*,#6371,.T.);
#9153=ORIENTED_EDGE('',*,*,#6405,.T.);
#9154=ORIENTED_EDGE('',*,*,#6406,.F.);
#9155=ORIENTED_EDGE('',*,*,#6407,.T.);
#9156=ORIENTED_EDGE('',*,*,#6389,.F.);
#9157=ORIENTED_EDGE('',*,*,#6408,.T.);
#9158=ORIENTED_EDGE('',*,*,#6406,.T.);
#9159=ORIENTED_EDGE('',*,*,#6409,.T.);
#9160=ORIENTED_EDGE('',*,*,#6369,.T.);
#9161=ORIENTED_EDGE('',*,*,#6410,.T.);
#9162=ORIENTED_EDGE('',*,*,#6411,.F.);
#9163=ORIENTED_EDGE('',*,*,#6412,.T.);
#9164=ORIENTED_EDGE('',*,*,#6391,.F.);
#9165=ORIENTED_EDGE('',*,*,#6413,.T.);
#9166=ORIENTED_EDGE('',*,*,#6411,.T.);
#9167=ORIENTED_EDGE('',*,*,#6414,.T.);
#9168=ORIENTED_EDGE('',*,*,#6367,.T.);
#9169=ORIENTED_EDGE('',*,*,#6415,.T.);
#9170=ORIENTED_EDGE('',*,*,#6416,.F.);
#9171=ORIENTED_EDGE('',*,*,#6417,.T.);
#9172=ORIENTED_EDGE('',*,*,#6381,.F.);
#9173=ORIENTED_EDGE('',*,*,#6418,.T.);
#9174=ORIENTED_EDGE('',*,*,#6416,.T.);
#9175=ORIENTED_EDGE('',*,*,#6419,.T.);
#9176=ORIENTED_EDGE('',*,*,#6377,.T.);
#9177=ORIENTED_EDGE('',*,*,#6420,.T.);
#9178=ORIENTED_EDGE('',*,*,#6393,.F.);
#9179=ORIENTED_EDGE('',*,*,#6421,.T.);
#9180=ORIENTED_EDGE('',*,*,#6383,.F.);
#9181=ORIENTED_EDGE('',*,*,#6422,.T.);
#9182=ORIENTED_EDGE('',*,*,#6422,.F.);
#9183=ORIENTED_EDGE('',*,*,#6382,.T.);
#9184=ORIENTED_EDGE('',*,*,#6417,.F.);
#9185=ORIENTED_EDGE('',*,*,#6384,.T.);
#9186=ORIENTED_EDGE('',*,*,#6421,.F.);
#9187=ORIENTED_EDGE('',*,*,#6398,.F.);
#9188=ORIENTED_EDGE('',*,*,#6403,.F.);
#9189=ORIENTED_EDGE('',*,*,#6386,.T.);
#9190=ORIENTED_EDGE('',*,*,#6397,.F.);
#9191=ORIENTED_EDGE('',*,*,#6408,.F.);
#9192=ORIENTED_EDGE('',*,*,#6388,.T.);
#9193=ORIENTED_EDGE('',*,*,#6402,.F.);
#9194=ORIENTED_EDGE('',*,*,#6413,.F.);
#9195=ORIENTED_EDGE('',*,*,#6390,.T.);
#9196=ORIENTED_EDGE('',*,*,#6407,.F.);
#9197=ORIENTED_EDGE('',*,*,#6418,.F.);
#9198=ORIENTED_EDGE('',*,*,#6380,.T.);
#9199=ORIENTED_EDGE('',*,*,#6412,.F.);
#9200=ORIENTED_EDGE('',*,*,#6378,.F.);
#9201=ORIENTED_EDGE('',*,*,#6419,.F.);
#9202=ORIENTED_EDGE('',*,*,#6415,.F.);
#9203=ORIENTED_EDGE('',*,*,#6420,.F.);
#9204=ORIENTED_EDGE('',*,*,#6376,.F.);
#9205=ORIENTED_EDGE('',*,*,#6394,.F.);
#9206=ORIENTED_EDGE('',*,*,#6374,.F.);
#9207=ORIENTED_EDGE('',*,*,#6399,.F.);
#9208=ORIENTED_EDGE('',*,*,#6395,.F.);
#9209=ORIENTED_EDGE('',*,*,#6372,.F.);
#9210=ORIENTED_EDGE('',*,*,#6404,.F.);
#9211=ORIENTED_EDGE('',*,*,#6400,.F.);
#9212=ORIENTED_EDGE('',*,*,#6370,.F.);
#9213=ORIENTED_EDGE('',*,*,#6409,.F.);
#9214=ORIENTED_EDGE('',*,*,#6405,.F.);
#9215=ORIENTED_EDGE('',*,*,#6368,.F.);
#9216=ORIENTED_EDGE('',*,*,#6414,.F.);
#9217=ORIENTED_EDGE('',*,*,#6410,.F.);
#9218=ORIENTED_EDGE('',*,*,#6392,.T.);
#9219=ORIENTED_EDGE('',*,*,#6423,.T.);
#9220=ORIENTED_EDGE('',*,*,#6379,.T.);
#9221=ORIENTED_EDGE('',*,*,#6423,.F.);
#9222=CYLINDRICAL_SURFACE('',#10269,18.);
#9223=CYLINDRICAL_SURFACE('',#10272,18.);
#9224=CYLINDRICAL_SURFACE('',#10275,18.);
#9225=CYLINDRICAL_SURFACE('',#10278,18.);
#9226=CYLINDRICAL_SURFACE('',#10281,18.);
#9227=CYLINDRICAL_SURFACE('',#10284,18.);
#9228=CYLINDRICAL_SURFACE('',#10287,18.);
#9229=CYLINDRICAL_SURFACE('',#10290,18.);
#9230=CYLINDRICAL_SURFACE('',#10293,18.);
#9231=CYLINDRICAL_SURFACE('',#10296,18.);
#9232=CYLINDRICAL_SURFACE('',#10299,18.);
#9233=CYLINDRICAL_SURFACE('',#10302,18.);
#9234=CYLINDRICAL_SURFACE('',#10305,18.);
#9235=CYLINDRICAL_SURFACE('',#10308,18.);
#9236=CYLINDRICAL_SURFACE('',#10311,18.);
#9237=CYLINDRICAL_SURFACE('',#10314,18.);
#9238=CYLINDRICAL_SURFACE('',#10317,18.);
#9239=CYLINDRICAL_SURFACE('',#10320,18.);
#9240=CYLINDRICAL_SURFACE('',#10323,18.);
#9241=CYLINDRICAL_SURFACE('',#10326,18.);
#9242=CYLINDRICAL_SURFACE('',#10329,18.);
#9243=CYLINDRICAL_SURFACE('',#10332,18.);
#9244=CYLINDRICAL_SURFACE('',#10335,18.);
#9245=CYLINDRICAL_SURFACE('',#10338,18.);
#9246=CYLINDRICAL_SURFACE('',#10341,18.);
#9247=CYLINDRICAL_SURFACE('',#10344,18.);
#9248=CYLINDRICAL_SURFACE('',#10347,18.);
#9249=CYLINDRICAL_SURFACE('',#10350,18.);
#9250=CYLINDRICAL_SURFACE('',#10353,18.);
#9251=CYLINDRICAL_SURFACE('',#10356,18.);
#9252=CYLINDRICAL_SURFACE('',#10359,18.);
#9253=CYLINDRICAL_SURFACE('',#10362,18.);
#9254=CYLINDRICAL_SURFACE('',#10365,18.);
#9255=CYLINDRICAL_SURFACE('',#10368,18.);
#9256=CYLINDRICAL_SURFACE('',#10371,18.);
#9257=CYLINDRICAL_SURFACE('',#10374,18.);
#9258=CYLINDRICAL_SURFACE('',#10377,18.);
#9259=CYLINDRICAL_SURFACE('',#10380,18.);
#9260=CYLINDRICAL_SURFACE('',#10383,18.);
#9261=CYLINDRICAL_SURFACE('',#10386,18.);
#9262=CYLINDRICAL_SURFACE('',#10469,25.);
#9263=CYLINDRICAL_SURFACE('',#10477,10.75);
#9264=CYLINDRICAL_SURFACE('',#10487,20.);
#9265=CYLINDRICAL_SURFACE('',#10502,8.35);
#9266=CYLINDRICAL_SURFACE('',#10511,3.10000000000001);
#9267=CYLINDRICAL_SURFACE('',#10529,17.85);
#9268=CYLINDRICAL_SURFACE('',#10537,20.);
#9269=CYLINDRICAL_SURFACE('',#10542,15.);
#9270=CYLINDRICAL_SURFACE('',#10550,16.5);
#9271=CYLINDRICAL_SURFACE('',#10555,17.85);
#9272=CYLINDRICAL_SURFACE('',#10556,3.);
#9273=CYLINDRICAL_SURFACE('',#10558,5.);
#9274=CYLINDRICAL_SURFACE('',#10571,3.);
#9275=CYLINDRICAL_SURFACE('',#10572,2.8);
#9276=CYLINDRICAL_SURFACE('',#10581,17.1);
#9277=CYLINDRICAL_SURFACE('',#10584,9.);
#9278=CYLINDRICAL_SURFACE('',#10593,3.);
#9279=CYLINDRICAL_SURFACE('',#10616,3.);
#9280=CYLINDRICAL_SURFACE('',#10629,5.);
#9281=CYLINDRICAL_SURFACE('',#10635,15.);
#9282=CYLINDRICAL_SURFACE('',#10646,12.5);
#9283=CYLINDRICAL_SURFACE('',#10649,12.5);
#9284=CYLINDRICAL_SURFACE('',#10657,2.8);
#9285=CYLINDRICAL_SURFACE('',#10662,1.);
#9286=CYLINDRICAL_SURFACE('',#10663,1.);
#9287=CYLINDRICAL_SURFACE('',#10664,1.);
#9288=CYLINDRICAL_SURFACE('',#10665,1.);
#9289=CYLINDRICAL_SURFACE('',#10705,11.1);
#9290=CYLINDRICAL_SURFACE('',#10708,11.1);
#9291=CYLINDRICAL_SURFACE('',#10711,11.1);
#9292=CYLINDRICAL_SURFACE('',#10721,9.2);
#9293=CYLINDRICAL_SURFACE('',#10725,3.09999999999999);
#9294=CYLINDRICAL_SURFACE('',#10726,3.09999999999999);
#9295=CYLINDRICAL_SURFACE('',#10727,2.);
#9296=CYLINDRICAL_SURFACE('',#10728,2.);
#9297=CYLINDRICAL_SURFACE('',#10734,1.865);
#9298=CYLINDRICAL_SURFACE('',#10737,1.865);
#9299=CYLINDRICAL_SURFACE('',#10740,1.865);
#9300=CYLINDRICAL_SURFACE('',#10743,1.865);
#9301=CYLINDRICAL_SURFACE('',#10746,1.865);
#9302=CYLINDRICAL_SURFACE('',#10749,1.865);
#9303=CYLINDRICAL_SURFACE('',#10752,1.865);
#9304=CYLINDRICAL_SURFACE('',#10755,1.865);
#9305=CYLINDRICAL_SURFACE('',#10758,1.865);
#9306=CYLINDRICAL_SURFACE('',#10761,1.865);
#9307=CYLINDRICAL_SURFACE('',#10768,9.1);
#9308=CYLINDRICAL_SURFACE('',#10775,2.125);
#9309=CYLINDRICAL_SURFACE('',#10778,2.125);
#9310=CYLINDRICAL_SURFACE('',#10781,3.5);
#9311=CYLINDRICAL_SURFACE('',#10786,5.);
#9312=CYLINDRICAL_SURFACE('',#10795,3.);
#9313=CYLINDRICAL_SURFACE('',#10815,9.15);
#9314=CYLINDRICAL_SURFACE('',#10824,6.75);
#9315=CYLINDRICAL_SURFACE('',#10876,8.925);
#9316=CYLINDRICAL_SURFACE('',#10888,9.15);
#9317=CYLINDRICAL_SURFACE('',#10889,7.25);
#9318=CYLINDRICAL_SURFACE('',#10905,3.);
#9319=CYLINDRICAL_SURFACE('',#10910,3.75);
#9320=CYLINDRICAL_SURFACE('',#10916,2.4);
#9321=CYLINDRICAL_SURFACE('',#10921,3.);
#9322=CYLINDRICAL_SURFACE('',#10924,17.5);
#9323=CYLINDRICAL_SURFACE('',#10927,17.5);
#9324=CYLINDRICAL_SURFACE('',#10930,17.5);
#9325=CYLINDRICAL_SURFACE('',#10933,17.5);
#9326=CYLINDRICAL_SURFACE('',#10937,17.5);
#9327=CYLINDRICAL_SURFACE('',#10940,17.5);
#9328=CYLINDRICAL_SURFACE('',#10943,17.5);
#9329=CYLINDRICAL_SURFACE('',#10946,17.5);
#9330=CYLINDRICAL_SURFACE('',#10949,17.5);
#9331=CYLINDRICAL_SURFACE('',#10965,14.);
#9332=CYLINDRICAL_SURFACE('',#10968,14.);
#9333=CYLINDRICAL_SURFACE('',#10971,17.5);
#9334=CYLINDRICAL_SURFACE('',#10979,13.);
#9335=CYLINDRICAL_SURFACE('',#10983,16.);
#9336=CYLINDRICAL_SURFACE('',#10989,11.35);
#9337=CYLINDRICAL_SURFACE('',#10990,1.87499999999999);
#9338=CYLINDRICAL_SURFACE('',#10991,1.87500000000001);
#9339=CYLINDRICAL_SURFACE('',#10992,1.875);
#9340=CYLINDRICAL_SURFACE('',#10993,1.875);
#9341=CYLINDRICAL_SURFACE('',#10994,1.875);
#9342=CYLINDRICAL_SURFACE('',#10995,15.);
#9343=CYLINDRICAL_SURFACE('',#11000,15.5);
#9344=CYLINDRICAL_SURFACE('',#11003,4.48804347826086);
#9345=CYLINDRICAL_SURFACE('',#11005,4.48804347826086);
#9346=CYLINDRICAL_SURFACE('',#11007,4.48804347826086);
#9347=CYLINDRICAL_SURFACE('',#11009,4.48804347826086);
#9348=CYLINDRICAL_SURFACE('',#11011,4.48804347826086);
#9349=CYLINDRICAL_SURFACE('',#11013,4.48804347826086);
#9350=CYLINDRICAL_SURFACE('',#11015,4.48804347826086);
#9351=CYLINDRICAL_SURFACE('',#11017,4.48804347826086);
#9352=CYLINDRICAL_SURFACE('',#11019,4.48804347826086);
#9353=CYLINDRICAL_SURFACE('',#11021,4.48804347826087);
#9354=CYLINDRICAL_SURFACE('',#11024,0.5);
#9355=CYLINDRICAL_SURFACE('',#11025,0.5);
#9356=CYLINDRICAL_SURFACE('',#11028,0.5);
#9357=CYLINDRICAL_SURFACE('',#11029,0.5);
#9358=CYLINDRICAL_SURFACE('',#11031,0.5);
#9359=CYLINDRICAL_SURFACE('',#11032,0.5);
#9360=CYLINDRICAL_SURFACE('',#11035,0.5);
#9361=CYLINDRICAL_SURFACE('',#11036,0.5);
#9362=CYLINDRICAL_SURFACE('',#11038,0.5);
#9363=CYLINDRICAL_SURFACE('',#11039,0.5);
#9364=CYLINDRICAL_SURFACE('',#11042,0.5);
#9365=CYLINDRICAL_SURFACE('',#11043,0.5);
#9366=CYLINDRICAL_SURFACE('',#11046,0.5);
#9367=CYLINDRICAL_SURFACE('',#11047,0.5);
#9368=CYLINDRICAL_SURFACE('',#11049,0.5);
#9369=CYLINDRICAL_SURFACE('',#11050,0.5);
#9370=CYLINDRICAL_SURFACE('',#11053,0.5);
#9371=CYLINDRICAL_SURFACE('',#11054,0.5);
#9372=CYLINDRICAL_SURFACE('',#11056,0.5);
#9373=CYLINDRICAL_SURFACE('',#11057,0.5);
#9374=CYLINDRICAL_SURFACE('',#11071,4.5);
#9375=CYLINDRICAL_SURFACE('',#11074,15.);
#9376=CYLINDRICAL_SURFACE('',#11117,19.);
#9377=CYLINDRICAL_SURFACE('',#11126,13.1);
#9378=CYLINDRICAL_SURFACE('',#11130,15.1);
#9379=CYLINDRICAL_SURFACE('',#11136,14.1);
#9380=CYLINDRICAL_SURFACE('',#11142,13.1);
#9381=CYLINDRICAL_SURFACE('',#11146,16.1);
#9382=CYLINDRICAL_SURFACE('',#11164,15.75);
#9383=CYLINDRICAL_SURFACE('',#11170,13.5);
#9384=CYLINDRICAL_SURFACE('',#11178,9.);
#9385=CYLINDRICAL_SURFACE('',#11222,3.5);
#9386=ADVANCED_FACE('',(#1020),#9222,.F.);
#9387=ADVANCED_FACE('',(#1021),#9223,.F.);
#9388=ADVANCED_FACE('',(#1022),#9224,.F.);
#9389=ADVANCED_FACE('',(#1023),#9225,.F.);
#9390=ADVANCED_FACE('',(#1024),#9226,.F.);
#9391=ADVANCED_FACE('',(#1025),#9227,.F.);
#9392=ADVANCED_FACE('',(#1026),#9228,.F.);
#9393=ADVANCED_FACE('',(#1027),#9229,.F.);
#9394=ADVANCED_FACE('',(#1028),#9230,.F.);
#9395=ADVANCED_FACE('',(#1029),#9231,.F.);
#9396=ADVANCED_FACE('',(#1030),#9232,.F.);
#9397=ADVANCED_FACE('',(#1031),#9233,.F.);
#9398=ADVANCED_FACE('',(#1032),#9234,.F.);
#9399=ADVANCED_FACE('',(#1033),#9235,.F.);
#9400=ADVANCED_FACE('',(#1034),#9236,.F.);
#9401=ADVANCED_FACE('',(#1035),#9237,.F.);
#9402=ADVANCED_FACE('',(#1036),#9238,.F.);
#9403=ADVANCED_FACE('',(#1037),#9239,.F.);
#9404=ADVANCED_FACE('',(#1038),#9240,.F.);
#9405=ADVANCED_FACE('',(#1039),#9241,.F.);
#9406=ADVANCED_FACE('',(#1040),#9242,.F.);
#9407=ADVANCED_FACE('',(#1041),#9243,.F.);
#9408=ADVANCED_FACE('',(#1042),#9244,.F.);
#9409=ADVANCED_FACE('',(#1043),#9245,.F.);
#9410=ADVANCED_FACE('',(#1044),#9246,.F.);
#9411=ADVANCED_FACE('',(#1045),#9247,.F.);
#9412=ADVANCED_FACE('',(#1046),#9248,.F.);
#9413=ADVANCED_FACE('',(#1047),#9249,.F.);
#9414=ADVANCED_FACE('',(#1048),#9250,.F.);
#9415=ADVANCED_FACE('',(#1049),#9251,.F.);
#9416=ADVANCED_FACE('',(#1050),#9252,.F.);
#9417=ADVANCED_FACE('',(#1051),#9253,.F.);
#9418=ADVANCED_FACE('',(#1052),#9254,.F.);
#9419=ADVANCED_FACE('',(#1053),#9255,.F.);
#9420=ADVANCED_FACE('',(#1054),#9256,.F.);
#9421=ADVANCED_FACE('',(#1055),#9257,.F.);
#9422=ADVANCED_FACE('',(#1056),#9258,.F.);
#9423=ADVANCED_FACE('',(#1057),#9259,.F.);
#9424=ADVANCED_FACE('',(#1058),#9260,.F.);
#9425=ADVANCED_FACE('',(#1059),#9261,.F.);
#9426=ADVANCED_FACE('',(#1060),#753,.F.);
#9427=ADVANCED_FACE('',(#1061),#754,.F.);
#9428=ADVANCED_FACE('',(#1062),#755,.F.);
#9429=ADVANCED_FACE('',(#1063),#756,.F.);
#9430=ADVANCED_FACE('',(#1064),#757,.F.);
#9431=ADVANCED_FACE('',(#1065),#758,.F.);
#9432=ADVANCED_FACE('',(#1066),#759,.F.);
#9433=ADVANCED_FACE('',(#1067),#760,.F.);
#9434=ADVANCED_FACE('',(#1068),#761,.F.);
#9435=ADVANCED_FACE('',(#1069),#762,.F.);
#9436=ADVANCED_FACE('',(#1070),#763,.F.);
#9437=ADVANCED_FACE('',(#1071),#764,.F.);
#9438=ADVANCED_FACE('',(#1072),#765,.F.);
#9439=ADVANCED_FACE('',(#1073),#766,.F.);
#9440=ADVANCED_FACE('',(#1074),#767,.F.);
#9441=ADVANCED_FACE('',(#1075),#768,.F.);
#9442=ADVANCED_FACE('',(#1076),#769,.F.);
#9443=ADVANCED_FACE('',(#1077),#770,.F.);
#9444=ADVANCED_FACE('',(#1078),#771,.F.);
#9445=ADVANCED_FACE('',(#1079),#772,.F.);
#9446=ADVANCED_FACE('',(#1080),#773,.F.);
#9447=ADVANCED_FACE('',(#1081),#774,.F.);
#9448=ADVANCED_FACE('',(#1082),#775,.F.);
#9449=ADVANCED_FACE('',(#1083),#776,.F.);
#9450=ADVANCED_FACE('',(#1084),#777,.F.);
#9451=ADVANCED_FACE('',(#1085),#778,.F.);
#9452=ADVANCED_FACE('',(#1086),#779,.F.);
#9453=ADVANCED_FACE('',(#1087),#780,.F.);
#9454=ADVANCED_FACE('',(#1088),#781,.F.);
#9455=ADVANCED_FACE('',(#1089),#782,.F.);
#9456=ADVANCED_FACE('',(#1090),#783,.F.);
#9457=ADVANCED_FACE('',(#1091),#784,.F.);
#9458=ADVANCED_FACE('',(#1092),#785,.F.);
#9459=ADVANCED_FACE('',(#1093),#786,.F.);
#9460=ADVANCED_FACE('',(#1094),#787,.F.);
#9461=ADVANCED_FACE('',(#1095),#788,.F.);
#9462=ADVANCED_FACE('',(#1096),#789,.F.);
#9463=ADVANCED_FACE('',(#1097),#790,.F.);
#9464=ADVANCED_FACE('',(#1098),#791,.F.);
#9465=ADVANCED_FACE('',(#1099),#792,.F.);
#9466=ADVANCED_FACE('',(#1100),#793,.F.);
#9467=ADVANCED_FACE('',(#1101),#794,.F.);
#9468=ADVANCED_FACE('',(#1102),#795,.F.);
#9469=ADVANCED_FACE('',(#1103),#796,.F.);
#9470=ADVANCED_FACE('',(#1104),#797,.F.);
#9471=ADVANCED_FACE('',(#1105),#798,.F.);
#9472=ADVANCED_FACE('',(#1106),#799,.F.);
#9473=ADVANCED_FACE('',(#1107),#800,.F.);
#9474=ADVANCED_FACE('',(#1108),#801,.F.);
#9475=ADVANCED_FACE('',(#1109),#802,.F.);
#9476=ADVANCED_FACE('',(#1110),#803,.F.);
#9477=ADVANCED_FACE('',(#1111),#804,.F.);
#9478=ADVANCED_FACE('',(#1112),#805,.F.);
#9479=ADVANCED_FACE('',(#1113),#806,.F.);
#9480=ADVANCED_FACE('',(#1114),#807,.F.);
#9481=ADVANCED_FACE('',(#1115),#808,.F.);
#9482=ADVANCED_FACE('',(#1116),#809,.F.);
#9483=ADVANCED_FACE('',(#1117),#810,.F.);
#9484=ADVANCED_FACE('',(#1118),#811,.F.);
#9485=ADVANCED_FACE('',(#1119),#812,.F.);
#9486=ADVANCED_FACE('',(#1120),#813,.F.);
#9487=ADVANCED_FACE('',(#1121),#814,.F.);
#9488=ADVANCED_FACE('',(#1122),#815,.F.);
#9489=ADVANCED_FACE('',(#1123),#816,.F.);
#9490=ADVANCED_FACE('',(#1124),#817,.F.);
#9491=ADVANCED_FACE('',(#1125),#818,.F.);
#9492=ADVANCED_FACE('',(#1126),#819,.F.);
#9493=ADVANCED_FACE('',(#1127),#820,.F.);
#9494=ADVANCED_FACE('',(#1128),#821,.F.);
#9495=ADVANCED_FACE('',(#1129),#822,.F.);
#9496=ADVANCED_FACE('',(#1130),#823,.F.);
#9497=ADVANCED_FACE('',(#1131),#824,.F.);
#9498=ADVANCED_FACE('',(#1132),#825,.F.);
#9499=ADVANCED_FACE('',(#1133),#826,.F.);
#9500=ADVANCED_FACE('',(#1134),#827,.F.);
#9501=ADVANCED_FACE('',(#1135),#828,.F.);
#9502=ADVANCED_FACE('',(#1136),#829,.F.);
#9503=ADVANCED_FACE('',(#1137),#830,.F.);
#9504=ADVANCED_FACE('',(#1138),#831,.F.);
#9505=ADVANCED_FACE('',(#1139),#832,.F.);
#9506=ADVANCED_FACE('',(#1140),#9262,.T.);
#9507=ADVANCED_FACE('',(#1141,#474),#833,.T.);
#9508=ADVANCED_FACE('',(#1142,#475),#834,.F.);
#9509=ADVANCED_FACE('',(#1143),#9263,.T.);
#9510=ADVANCED_FACE('',(#1144),#416,.F.);
#9511=ADVANCED_FACE('',(#1145),#417,.F.);
#9512=ADVANCED_FACE('',(#1146),#418,.F.);
#9513=ADVANCED_FACE('',(#1147),#419,.F.);
#9514=ADVANCED_FACE('',(#1148),#420,.F.);
#9515=ADVANCED_FACE('',(#1149),#421,.F.);
#9516=ADVANCED_FACE('',(#1150),#9264,.F.);
#9517=ADVANCED_FACE('',(#1151,#476),#835,.T.);
#9518=ADVANCED_FACE('',(#1152),#422,.T.);
#9519=ADVANCED_FACE('',(#1153),#423,.T.);
#9520=ADVANCED_FACE('',(#1154),#384,.T.);
#9521=ADVANCED_FACE('',(#1155),#424,.T.);
#9522=ADVANCED_FACE('',(#1156),#425,.T.);
#9523=ADVANCED_FACE('',(#1157),#426,.T.);
#9524=ADVANCED_FACE('',(#1158),#427,.T.);
#9525=ADVANCED_FACE('',(#1159),#385,.T.);
#9526=ADVANCED_FACE('',(#1160),#428,.T.);
#9527=ADVANCED_FACE('',(#1161),#429,.T.);
#9528=ADVANCED_FACE('',(#1162,#477),#836,.F.);
#9529=ADVANCED_FACE('',(#1163),#9265,.T.);
#9530=ADVANCED_FACE('',(#1164,#478,#479),#430,.F.);
#9531=ADVANCED_FACE('',(#1165),#345,.T.);
#9532=ADVANCED_FACE('',(#1166),#386,.F.);
#9533=ADVANCED_FACE('',(#1167),#9266,.F.);
#9534=ADVANCED_FACE('',(#1168,#480),#837,.F.);
#9535=ADVANCED_FACE('',(#1169),#838,.T.);
#9536=ADVANCED_FACE('',(#1170),#839,.F.);
#9537=ADVANCED_FACE('',(#1171),#840,.T.);
#9538=ADVANCED_FACE('',(#1172),#841,.F.);
#9539=ADVANCED_FACE('',(#1173),#842,.T.);
#9540=ADVANCED_FACE('',(#1174),#843,.F.);
#9541=ADVANCED_FACE('',(#1175),#844,.F.);
#9542=ADVANCED_FACE('',(#1176),#845,.F.);
#9543=ADVANCED_FACE('',(#1177),#846,.F.);
#9544=ADVANCED_FACE('',(#1178),#847,.F.);
#9545=ADVANCED_FACE('',(#1179),#848,.F.);
#9546=ADVANCED_FACE('',(#1180,#481),#849,.F.);
#9547=ADVANCED_FACE('',(#1181),#850,.F.);
#9548=ADVANCED_FACE('',(#1182),#9267,.T.);
#9549=ADVANCED_FACE('',(#1183,#482),#851,.T.);
#9550=ADVANCED_FACE('',(#1184),#9268,.T.);
#9551=ADVANCED_FACE('',(#1185,#483),#852,.T.);
#9552=ADVANCED_FACE('',(#1186),#9269,.F.);
#9553=ADVANCED_FACE('',(#1187,#484,#485),#853,.T.);
#9554=ADVANCED_FACE('',(#1188,#486),#854,.T.);
#9555=ADVANCED_FACE('',(#1189),#9270,.T.);
#9556=ADVANCED_FACE('',(#1190,#487),#855,.T.);
#9557=ADVANCED_FACE('',(#1191,#488),#856,.T.);
#9558=ADVANCED_FACE('',(#1192),#9271,.T.);
#9559=ADVANCED_FACE('',(#1193),#9272,.F.);
#9560=ADVANCED_FACE('',(#1194),#9273,.F.);
#9561=ADVANCED_FACE('',(#1195),#857,.T.);
#9562=ADVANCED_FACE('',(#1196,#489),#858,.F.);
#9563=ADVANCED_FACE('',(#1197),#859,.F.);
#9564=ADVANCED_FACE('',(#1198),#860,.F.);
#9565=ADVANCED_FACE('',(#1199,#490),#861,.F.);
#9566=ADVANCED_FACE('',(#1200),#862,.T.);
#9567=ADVANCED_FACE('',(#1201),#9274,.F.);
#9568=ADVANCED_FACE('',(#1202),#9275,.F.);
#9569=ADVANCED_FACE('',(#1203),#863,.T.);
#9570=ADVANCED_FACE('',(#1204),#346,.T.);
#9571=ADVANCED_FACE('',(#1205),#864,.F.);
#9572=ADVANCED_FACE('',(#1206),#347,.T.);
#9573=ADVANCED_FACE('',(#1207),#348,.F.);
#9574=ADVANCED_FACE('',(#1208),#9276,.T.);
#9575=ADVANCED_FACE('',(#1209),#9277,.F.);
#9576=ADVANCED_FACE('',(#1210),#865,.F.);
#9577=ADVANCED_FACE('',(#1211),#866,.F.);
#9578=ADVANCED_FACE('',(#1212,#491),#867,.T.);
#9579=ADVANCED_FACE('',(#1213,#492),#868,.F.);
#9580=ADVANCED_FACE('',(#1214),#9278,.F.);
#9581=ADVANCED_FACE('',(#1215),#869,.T.);
#9582=ADVANCED_FACE('',(#1216),#870,.T.);
#9583=ADVANCED_FACE('',(#1217),#871,.T.);
#9584=ADVANCED_FACE('',(#1218),#872,.T.);
#9585=ADVANCED_FACE('',(#1219),#873,.T.);
#9586=ADVANCED_FACE('',(#1220),#874,.T.);
#9587=ADVANCED_FACE('',(#1221),#875,.T.);
#9588=ADVANCED_FACE('',(#1222),#876,.T.);
#9589=ADVANCED_FACE('',(#1223),#877,.F.);
#9590=ADVANCED_FACE('',(#1224),#878,.F.);
#9591=ADVANCED_FACE('',(#1225),#879,.F.);
#9592=ADVANCED_FACE('',(#1226),#880,.F.);
#9593=ADVANCED_FACE('',(#1227),#881,.F.);
#9594=ADVANCED_FACE('',(#1228),#882,.F.);
#9595=ADVANCED_FACE('',(#1229),#883,.F.);
#9596=ADVANCED_FACE('',(#1230),#884,.F.);
#9597=ADVANCED_FACE('',(#1231),#349,.F.);
#9598=ADVANCED_FACE('',(#1232),#350,.F.);
#9599=ADVANCED_FACE('',(#1233),#9279,.T.);
#9600=ADVANCED_FACE('',(#1234),#885,.T.);
#9601=ADVANCED_FACE('',(#1235),#886,.F.);
#9602=ADVANCED_FACE('',(#1236),#351,.T.);
#9603=ADVANCED_FACE('',(#1237),#352,.T.);
#9604=ADVANCED_FACE('',(#1238),#887,.T.);
#9605=ADVANCED_FACE('',(#1239,#493),#9280,.T.);
#9606=ADVANCED_FACE('',(#1240,#494),#888,.T.);
#9607=ADVANCED_FACE('',(#1241),#9281,.T.);
#9608=ADVANCED_FACE('',(#1242,#495),#889,.T.);
#9609=ADVANCED_FACE('',(#1243),#9282,.T.);
#9610=ADVANCED_FACE('',(#1244),#890,.F.);
#9611=ADVANCED_FACE('',(#1245),#9283,.T.);
#9612=ADVANCED_FACE('',(#1246),#891,.F.);
#9613=ADVANCED_FACE('',(#1247),#892,.T.);
#9614=ADVANCED_FACE('',(#1248),#9284,.F.);
#9615=ADVANCED_FACE('',(#1249),#893,.T.);
#9616=ADVANCED_FACE('',(#1250),#353,.T.);
#9617=ADVANCED_FACE('',(#1251),#354,.T.);
#9618=ADVANCED_FACE('',(#1252),#9285,.T.);
#9619=ADVANCED_FACE('',(#1253),#9286,.T.);
#9620=ADVANCED_FACE('',(#1254),#9287,.T.);
#9621=ADVANCED_FACE('',(#1255),#9288,.T.);
#9622=ADVANCED_FACE('',(#1256),#431,.F.);
#9623=ADVANCED_FACE('',(#1257),#432,.F.);
#9624=ADVANCED_FACE('',(#1258),#433,.F.);
#9625=ADVANCED_FACE('',(#1259),#434,.F.);
#9626=ADVANCED_FACE('',(#1260),#894,.F.);
#9627=ADVANCED_FACE('',(#1261),#895,.T.);
#9628=ADVANCED_FACE('',(#1262),#435,.F.);
#9629=ADVANCED_FACE('',(#1263),#436,.F.);
#9630=ADVANCED_FACE('',(#1264),#437,.F.);
#9631=ADVANCED_FACE('',(#1265),#438,.F.);
#9632=ADVANCED_FACE('',(#1266),#896,.F.);
#9633=ADVANCED_FACE('',(#1267),#897,.T.);
#9634=ADVANCED_FACE('',(#1268),#177,.T.);
#9635=ADVANCED_FACE('',(#1269),#387,.T.);
#9636=ADVANCED_FACE('',(#1270,#496,#497,#498,#499,#500,#501,#502,#503,#504),
#9289,.T.);
#9637=ADVANCED_FACE('',(#1271,#505),#9290,.T.);
#9638=ADVANCED_FACE('',(#1272,#506),#9291,.T.);
#9639=ADVANCED_FACE('',(#1273,#507),#898,.T.);
#9640=ADVANCED_FACE('',(#1274,#508),#899,.F.);
#9641=ADVANCED_FACE('',(#1275,#509,#510),#9292,.F.);
#9642=ADVANCED_FACE('',(#1276),#9293,.F.);
#9643=ADVANCED_FACE('',(#1277),#9294,.F.);
#9644=ADVANCED_FACE('',(#1278),#9295,.F.);
#9645=ADVANCED_FACE('',(#1279),#9296,.F.);
#9646=ADVANCED_FACE('',(#1280),#388,.F.);
#9647=ADVANCED_FACE('',(#1281),#389,.F.);
#9648=ADVANCED_FACE('',(#1282),#439,.T.);
#9649=ADVANCED_FACE('',(#1283),#9297,.F.);
#9650=ADVANCED_FACE('',(#1284),#440,.T.);
#9651=ADVANCED_FACE('',(#1285),#441,.T.);
#9652=ADVANCED_FACE('',(#1286),#9298,.F.);
#9653=ADVANCED_FACE('',(#1287),#442,.T.);
#9654=ADVANCED_FACE('',(#1288),#443,.T.);
#9655=ADVANCED_FACE('',(#1289),#9299,.F.);
#9656=ADVANCED_FACE('',(#1290),#444,.T.);
#9657=ADVANCED_FACE('',(#1291),#445,.T.);
#9658=ADVANCED_FACE('',(#1292),#9300,.F.);
#9659=ADVANCED_FACE('',(#1293),#446,.T.);
#9660=ADVANCED_FACE('',(#1294),#447,.T.);
#9661=ADVANCED_FACE('',(#1295),#9301,.F.);
#9662=ADVANCED_FACE('',(#1296),#448,.T.);
#9663=ADVANCED_FACE('',(#1297),#449,.T.);
#9664=ADVANCED_FACE('',(#1298),#9302,.F.);
#9665=ADVANCED_FACE('',(#1299),#450,.T.);
#9666=ADVANCED_FACE('',(#1300),#451,.T.);
#9667=ADVANCED_FACE('',(#1301),#9303,.F.);
#9668=ADVANCED_FACE('',(#1302),#452,.T.);
#9669=ADVANCED_FACE('',(#1303),#453,.T.);
#9670=ADVANCED_FACE('',(#1304),#9304,.F.);
#9671=ADVANCED_FACE('',(#1305),#454,.T.);
#9672=ADVANCED_FACE('',(#1306),#455,.T.);
#9673=ADVANCED_FACE('',(#1307),#9305,.F.);
#9674=ADVANCED_FACE('',(#1308),#456,.T.);
#9675=ADVANCED_FACE('',(#1309),#457,.T.);
#9676=ADVANCED_FACE('',(#1310),#9306,.F.);
#9677=ADVANCED_FACE('',(#1311),#458,.T.);
#9678=ADVANCED_FACE('',(#1312),#11,.T.);
#9679=ADVANCED_FACE('',(#1313),#12,.T.);
#9680=ADVANCED_FACE('',(#1314),#355,.F.);
#9681=ADVANCED_FACE('',(#1315),#356,.F.);
#9682=ADVANCED_FACE('',(#1316),#357,.T.);
#9683=ADVANCED_FACE('',(#1317),#358,.T.);
#9684=ADVANCED_FACE('',(#1318,#511),#9307,.T.);
#9685=ADVANCED_FACE('',(#1319,#512),#900,.T.);
#9686=ADVANCED_FACE('',(#1320,#513),#901,.F.);
#9687=ADVANCED_FACE('',(#1321),#9308,.F.);
#9688=ADVANCED_FACE('',(#1322),#902,.T.);
#9689=ADVANCED_FACE('',(#1323),#9309,.F.);
#9690=ADVANCED_FACE('',(#1324),#903,.T.);
#9691=ADVANCED_FACE('',(#1325),#9310,.F.);
#9692=ADVANCED_FACE('',(#1326,#514),#904,.F.);
#9693=ADVANCED_FACE('',(#1327),#9311,.T.);
#9694=ADVANCED_FACE('',(#1328,#515),#905,.F.);
#9695=ADVANCED_FACE('',(#1329),#178,.T.);
#9696=ADVANCED_FACE('',(#1330),#390,.T.);
#9697=ADVANCED_FACE('',(#1331),#9312,.T.);
#9698=ADVANCED_FACE('',(#1332),#359,.T.);
#9699=ADVANCED_FACE('',(#1333),#906,.T.);
#9700=ADVANCED_FACE('',(#1334),#907,.F.);
#9701=ADVANCED_FACE('',(#1335),#908,.F.);
#9702=ADVANCED_FACE('',(#1336),#909,.F.);
#9703=ADVANCED_FACE('',(#1337),#910,.F.);
#9704=ADVANCED_FACE('',(#1338),#911,.F.);
#9705=ADVANCED_FACE('',(#1339),#912,.F.);
#9706=ADVANCED_FACE('',(#1340,#516),#913,.F.);
#9707=ADVANCED_FACE('',(#1341),#914,.F.);
#9708=ADVANCED_FACE('',(#1342),#915,.T.);
#9709=ADVANCED_FACE('',(#1343),#459,.F.);
#9710=ADVANCED_FACE('',(#1344),#916,.F.);
#9711=ADVANCED_FACE('',(#1345),#917,.F.);
#9712=ADVANCED_FACE('',(#1346),#9313,.T.);
#9713=ADVANCED_FACE('',(#1347,#517),#918,.T.);
#9714=ADVANCED_FACE('',(#1348,#518),#919,.F.);
#9715=ADVANCED_FACE('',(#1349),#9314,.T.);
#9716=ADVANCED_FACE('',(#1350,#519),#920,.T.);
#9717=ADVANCED_FACE('',(#1351),#921,.F.);
#9718=ADVANCED_FACE('',(#1352),#922,.T.);
#9719=ADVANCED_FACE('',(#1353),#923,.F.);
#9720=ADVANCED_FACE('',(#1354),#924,.T.);
#9721=ADVANCED_FACE('',(#1355),#925,.T.);
#9722=ADVANCED_FACE('',(#1356),#391,.T.);
#9723=ADVANCED_FACE('',(#1357),#179,.F.);
#9724=ADVANCED_FACE('',(#1358,#520),#926,.F.);
#9725=ADVANCED_FACE('',(#1359),#927,.F.);
#9726=ADVANCED_FACE('',(#1360),#928,.F.);
#9727=ADVANCED_FACE('',(#1361),#929,.F.);
#9728=ADVANCED_FACE('',(#1362),#930,.F.);
#9729=ADVANCED_FACE('',(#1363,#521),#931,.T.);
#9730=ADVANCED_FACE('',(#1364),#932,.T.);
#9731=ADVANCED_FACE('',(#1365),#933,.T.);
#9732=ADVANCED_FACE('',(#1366),#934,.T.);
#9733=ADVANCED_FACE('',(#1367),#935,.T.);
#9734=ADVANCED_FACE('',(#1368),#936,.T.);
#9735=ADVANCED_FACE('',(#1369),#937,.T.);
#9736=ADVANCED_FACE('',(#1370),#938,.T.);
#9737=ADVANCED_FACE('',(#1371),#939,.T.);
#9738=ADVANCED_FACE('',(#1372),#940,.T.);
#9739=ADVANCED_FACE('',(#1373),#941,.T.);
#9740=ADVANCED_FACE('',(#1374),#942,.T.);
#9741=ADVANCED_FACE('',(#1375),#943,.T.);
#9742=ADVANCED_FACE('',(#1376),#944,.F.);
#9743=ADVANCED_FACE('',(#1377),#945,.F.);
#9744=ADVANCED_FACE('',(#1378),#946,.F.);
#9745=ADVANCED_FACE('',(#1379),#947,.F.);
#9746=ADVANCED_FACE('',(#1380),#948,.F.);
#9747=ADVANCED_FACE('',(#1381),#949,.F.);
#9748=ADVANCED_FACE('',(#1382),#950,.F.);
#9749=ADVANCED_FACE('',(#1383),#951,.F.);
#9750=ADVANCED_FACE('',(#1384),#952,.F.);
#9751=ADVANCED_FACE('',(#1385),#953,.F.);
#9752=ADVANCED_FACE('',(#1386),#954,.F.);
#9753=ADVANCED_FACE('',(#1387),#955,.F.);
#9754=ADVANCED_FACE('',(#1388),#956,.F.);
#9755=ADVANCED_FACE('',(#1389),#957,.F.);
#9756=ADVANCED_FACE('',(#1390),#392,.T.);
#9757=ADVANCED_FACE('',(#1391),#958,.T.);
#9758=ADVANCED_FACE('',(#1392),#959,.F.);
#9759=ADVANCED_FACE('',(#1393),#9315,.T.);
#9760=ADVANCED_FACE('',(#1394),#960,.T.);
#9761=ADVANCED_FACE('',(#1395),#961,.F.);
#9762=ADVANCED_FACE('',(#1396,#522),#962,.T.);
#9763=ADVANCED_FACE('',(#1397,#523),#963,.F.);
#9764=ADVANCED_FACE('',(#1398),#9316,.T.);
#9765=ADVANCED_FACE('',(#1399),#9317,.F.);
#9766=ADVANCED_FACE('',(#1400),#9318,.T.);
#9767=ADVANCED_FACE('',(#1401,#524),#964,.F.);
#9768=ADVANCED_FACE('',(#1402),#9319,.T.);
#9769=ADVANCED_FACE('',(#1403),#965,.F.);
#9770=ADVANCED_FACE('',(#1404,#525),#966,.T.);
#9771=ADVANCED_FACE('',(#1405),#9320,.T.);
#9772=ADVANCED_FACE('',(#1406,#526),#967,.T.);
#9773=ADVANCED_FACE('',(#1407),#968,.F.);
#9774=ADVANCED_FACE('',(#1408),#9321,.T.);
#9775=ADVANCED_FACE('',(#1409),#9322,.T.);
#9776=ADVANCED_FACE('',(#1410),#9323,.T.);
#9777=ADVANCED_FACE('',(#1411),#9324,.T.);
#9778=ADVANCED_FACE('',(#1412),#9325,.T.);
#9779=ADVANCED_FACE('',(#1413),#9326,.T.);
#9780=ADVANCED_FACE('',(#1414),#9327,.T.);
#9781=ADVANCED_FACE('',(#1415),#9328,.T.);
#9782=ADVANCED_FACE('',(#1416),#9329,.T.);
#9783=ADVANCED_FACE('',(#1417),#9330,.T.);
#9784=ADVANCED_FACE('',(#1418,#527),#969,.F.);
#9785=ADVANCED_FACE('',(#1419),#9331,.F.);
#9786=ADVANCED_FACE('',(#1420),#9332,.F.);
#9787=ADVANCED_FACE('',(#1421),#9333,.T.);
#9788=ADVANCED_FACE('',(#1422,#528),#970,.F.);
#9789=ADVANCED_FACE('',(#1423),#360,.T.);
#9790=ADVANCED_FACE('',(#1424,#529,#530,#531,#532,#533),#9334,.T.);
#9791=ADVANCED_FACE('',(#1425,#534),#971,.F.);
#9792=ADVANCED_FACE('',(#1426),#9335,.T.);
#9793=ADVANCED_FACE('',(#1427),#361,.T.);
#9794=ADVANCED_FACE('',(#1428,#535),#972,.F.);
#9795=ADVANCED_FACE('',(#1429,#536,#537,#538,#539,#540),#9336,.F.);
#9796=ADVANCED_FACE('',(#1430),#9337,.F.);
#9797=ADVANCED_FACE('',(#1431),#9338,.F.);
#9798=ADVANCED_FACE('',(#1432),#9339,.F.);
#9799=ADVANCED_FACE('',(#1433),#9340,.F.);
#9800=ADVANCED_FACE('',(#1434),#9341,.F.);
#9801=ADVANCED_FACE('',(#1435),#9342,.F.);
#9802=ADVANCED_FACE('',(#1436),#362,.F.);
#9803=ADVANCED_FACE('',(#1437,#541),#973,.T.);
#9804=ADVANCED_FACE('',(#1438),#9343,.F.);
#9805=ADVANCED_FACE('',(#1439,#542),#974,.T.);
#9806=ADVANCED_FACE('',(#1440),#9344,.F.);
#9807=ADVANCED_FACE('',(#1441),#9345,.F.);
#9808=ADVANCED_FACE('',(#1442),#9346,.F.);
#9809=ADVANCED_FACE('',(#1443),#9347,.F.);
#9810=ADVANCED_FACE('',(#1444),#9348,.F.);
#9811=ADVANCED_FACE('',(#1445),#9349,.F.);
#9812=ADVANCED_FACE('',(#1446),#9350,.F.);
#9813=ADVANCED_FACE('',(#1447),#9351,.F.);
#9814=ADVANCED_FACE('',(#1448),#9352,.F.);
#9815=ADVANCED_FACE('',(#1449),#9353,.F.);
#9816=ADVANCED_FACE('',(#1450),#460,.T.);
#9817=ADVANCED_FACE('',(#1451),#9354,.T.);
#9818=ADVANCED_FACE('',(#1452),#9355,.T.);
#9819=ADVANCED_FACE('',(#1453),#393,.T.);
#9820=ADVANCED_FACE('',(#1454),#461,.T.);
#9821=ADVANCED_FACE('',(#1455),#9356,.T.);
#9822=ADVANCED_FACE('',(#1456),#9357,.T.);
#9823=ADVANCED_FACE('',(#1457),#394,.T.);
#9824=ADVANCED_FACE('',(#1458),#462,.T.);
#9825=ADVANCED_FACE('',(#1459),#9358,.T.);
#9826=ADVANCED_FACE('',(#1460),#9359,.T.);
#9827=ADVANCED_FACE('',(#1461),#395,.T.);
#9828=ADVANCED_FACE('',(#1462),#463,.T.);
#9829=ADVANCED_FACE('',(#1463),#9360,.T.);
#9830=ADVANCED_FACE('',(#1464),#9361,.T.);
#9831=ADVANCED_FACE('',(#1465),#396,.T.);
#9832=ADVANCED_FACE('',(#1466),#464,.T.);
#9833=ADVANCED_FACE('',(#1467),#9362,.T.);
#9834=ADVANCED_FACE('',(#1468),#9363,.T.);
#9835=ADVANCED_FACE('',(#1469),#397,.T.);
#9836=ADVANCED_FACE('',(#1470),#465,.T.);
#9837=ADVANCED_FACE('',(#1471),#9364,.T.);
#9838=ADVANCED_FACE('',(#1472),#9365,.T.);
#9839=ADVANCED_FACE('',(#1473),#398,.T.);
#9840=ADVANCED_FACE('',(#1474),#466,.T.);
#9841=ADVANCED_FACE('',(#1475),#9366,.T.);
#9842=ADVANCED_FACE('',(#1476),#9367,.T.);
#9843=ADVANCED_FACE('',(#1477),#399,.T.);
#9844=ADVANCED_FACE('',(#1478),#467,.T.);
#9845=ADVANCED_FACE('',(#1479),#9368,.T.);
#9846=ADVANCED_FACE('',(#1480),#9369,.T.);
#9847=ADVANCED_FACE('',(#1481),#400,.T.);
#9848=ADVANCED_FACE('',(#1482),#468,.T.);
#9849=ADVANCED_FACE('',(#1483),#9370,.T.);
#9850=ADVANCED_FACE('',(#1484),#9371,.T.);
#9851=ADVANCED_FACE('',(#1485),#401,.T.);
#9852=ADVANCED_FACE('',(#1486),#469,.T.);
#9853=ADVANCED_FACE('',(#1487),#9372,.T.);
#9854=ADVANCED_FACE('',(#1488),#9373,.T.);
#9855=ADVANCED_FACE('',(#1489),#402,.T.);
#9856=ADVANCED_FACE('',(#1490,#543),#975,.F.);
#9857=ADVANCED_FACE('',(#1491,#544),#976,.F.);
#9858=ADVANCED_FACE('',(#1492),#977,.F.);
#9859=ADVANCED_FACE('',(#1493),#978,.F.);
#9860=ADVANCED_FACE('',(#1494),#979,.F.);
#9861=ADVANCED_FACE('',(#1495),#980,.F.);
#9862=ADVANCED_FACE('',(#1496),#981,.F.);
#9863=ADVANCED_FACE('',(#1497),#982,.F.);
#9864=ADVANCED_FACE('',(#1498),#9374,.F.);
#9865=ADVANCED_FACE('',(#1499),#9375,.T.);
#9866=ADVANCED_FACE('',(#1500,#545),#983,.T.);
#9867=ADVANCED_FACE('',(#1501),#984,.F.);
#9868=ADVANCED_FACE('',(#1502),#985,.F.);
#9869=ADVANCED_FACE('',(#1503),#986,.F.);
#9870=ADVANCED_FACE('',(#1504),#987,.F.);
#9871=ADVANCED_FACE('',(#1505),#988,.F.);
#9872=ADVANCED_FACE('',(#1506),#989,.F.);
#9873=ADVANCED_FACE('',(#1507),#990,.F.);
#9874=ADVANCED_FACE('',(#1508),#991,.F.);
#9875=ADVANCED_FACE('',(#1509),#992,.F.);
#9876=ADVANCED_FACE('',(#1510),#993,.F.);
#9877=ADVANCED_FACE('',(#1511),#994,.F.);
#9878=ADVANCED_FACE('',(#1512),#995,.F.);
#9879=ADVANCED_FACE('',(#1513),#996,.F.);
#9880=ADVANCED_FACE('',(#1514),#997,.F.);
#9881=ADVANCED_FACE('',(#1515),#998,.F.);
#9882=ADVANCED_FACE('',(#1516),#999,.F.);
#9883=ADVANCED_FACE('',(#1517),#1000,.F.);
#9884=ADVANCED_FACE('',(#1518),#1001,.F.);
#9885=ADVANCED_FACE('',(#1519),#363,.F.);
#9886=ADVANCED_FACE('',(#1520),#403,.T.);
#9887=ADVANCED_FACE('',(#1521),#364,.T.);
#9888=ADVANCED_FACE('',(#1522),#470,.F.);
#9889=ADVANCED_FACE('',(#1523),#471,.F.);
#9890=ADVANCED_FACE('',(#1524),#472,.F.);
#9891=ADVANCED_FACE('',(#1525),#473,.F.);
#9892=ADVANCED_FACE('',(#1526),#1002,.F.);
#9893=ADVANCED_FACE('',(#1527),#1003,.T.);
#9894=ADVANCED_FACE('',(#1528,#546),#1004,.F.);
#9895=ADVANCED_FACE('',(#1529),#9376,.T.);
#9896=ADVANCED_FACE('',(#1530),#404,.F.);
#9897=ADVANCED_FACE('',(#1531),#365,.T.);
#9898=ADVANCED_FACE('',(#1532,#547),#1005,.F.);
#9899=ADVANCED_FACE('',(#1533),#9377,.F.);
#9900=ADVANCED_FACE('',(#1534,#548),#1006,.F.);
#9901=ADVANCED_FACE('',(#1535),#9378,.F.);
#9902=ADVANCED_FACE('',(#1536),#366,.F.);
#9903=ADVANCED_FACE('',(#1537),#9379,.F.);
#9904=ADVANCED_FACE('',(#1538),#367,.F.);
#9905=ADVANCED_FACE('',(#1539),#9380,.F.);
#9906=ADVANCED_FACE('',(#1540,#549),#1007,.F.);
#9907=ADVANCED_FACE('',(#1541),#9381,.F.);
#9908=ADVANCED_FACE('',(#1542),#180,.T.);
#9909=ADVANCED_FACE('',(#1543),#1008,.F.);
#9910=ADVANCED_FACE('',(#1544),#368,.T.);
#9911=ADVANCED_FACE('',(#1545),#9382,.T.);
#9912=ADVANCED_FACE('',(#1546,#550),#1009,.F.);
#9913=ADVANCED_FACE('',(#1547),#9383,.T.);
#9914=ADVANCED_FACE('',(#1548),#369,.T.);
#9915=ADVANCED_FACE('',(#1549),#370,.T.);
#9916=ADVANCED_FACE('',(#1550),#1010,.T.);
#9917=ADVANCED_FACE('',(#1551),#9384,.F.);
#9918=ADVANCED_FACE('',(#1552),#371,.F.);
#9919=ADVANCED_FACE('',(#1553,#551),#1011,.F.);
#9920=ADVANCED_FACE('',(#1554),#405,.T.);
#9921=ADVANCED_FACE('',(#1555,#552),#1012,.F.);
#9922=ADVANCED_FACE('',(#1556,#553),#1013,.T.);
#9923=ADVANCED_FACE('',(#1557),#1014,.F.);
#9924=ADVANCED_FACE('',(#1558),#1015,.F.);
#9925=ADVANCED_FACE('',(#1559),#1016,.F.);
#9926=ADVANCED_FACE('',(#1560),#1017,.F.);
#9927=ADVANCED_FACE('',(#1561),#1018,.F.);
#9928=ADVANCED_FACE('',(#1562),#1019,.F.);
#9929=ADVANCED_FACE('',(#1563),#372,.T.);
#9930=ADVANCED_FACE('',(#1564),#373,.T.);
#9931=ADVANCED_FACE('',(#1565),#374,.T.);
#9932=ADVANCED_FACE('',(#1566),#375,.T.);
#9933=ADVANCED_FACE('',(#1567),#376,.T.);
#9934=ADVANCED_FACE('',(#1568),#377,.T.);
#9935=ADVANCED_FACE('',(#1569),#378,.T.);
#9936=ADVANCED_FACE('',(#1570),#379,.T.);
#9937=ADVANCED_FACE('',(#1571),#380,.T.);
#9938=ADVANCED_FACE('',(#1572),#381,.T.);
#9939=ADVANCED_FACE('',(#1573),#382,.T.);
#9940=ADVANCED_FACE('',(#1574),#383,.T.);
#9941=ADVANCED_FACE('',(#1575),#9385,.F.);
#9942=CLOSED_SHELL('',(#9386,#9387,#9388,#9389,#9390,#9391,#9392,#9393,
#9394,#9395,#9396,#9397,#9398,#9399,#9400,#9401,#9402,#9403,#9404,#9405,
#9406,#9407,#9408,#9409,#9410,#9411,#9412,#9413,#9414,#9415,#9416,#9417,
#9418,#9419,#9420,#9421,#9422,#9423,#9424,#9425,#9426,#9427,#9428,#9429,
#9430,#9431,#9432,#9433,#9434,#9435,#9436,#9437,#9438,#9439,#9440,#9441,
#9442,#9443,#9444,#9445,#9446,#9447,#9448,#9449,#9450,#9451,#9452,#9453,
#9454,#9455,#9456,#9457,#9458,#9459,#9460,#9461,#9462,#9463,#9464,#9465,
#9466,#9467,#9468,#9469,#9470,#9471,#9472,#9473,#9474,#9475,#9476,#9477,
#9478,#9479,#9480,#9481,#9482,#9483,#9484,#9485,#9486,#9487,#9488,#9489,
#9490,#9491,#9492,#9493,#9494,#9495,#9496,#9497,#9498,#9499,#9500,#9501,
#9502,#9503,#9504,#9505,#9506,#9507,#9508,#9509,#9510,#9511,#9512,#9513,
#9514,#9515,#9516,#9517,#9518,#9519,#9520,#9521,#9522,#9523,#9524,#9525,
#9526,#9527,#9528,#9529,#9530,#9531,#9532,#9533,#9534,#9535,#9536,#9537,
#9538,#9539));
#9943=CLOSED_SHELL('',(#9540,#9541,#9542,#9543,#9544,#9545,#9546,#9547,
#9548,#9549,#9550,#9551,#9552,#9553,#9554,#9555,#9556,#9557,#9558,#9559,
#9560,#9561,#9562,#9563,#9564,#9565,#9566,#9567,#9568,#9569,#9570,#9571,
#9572,#9573));
#9944=CLOSED_SHELL('',(#9574,#9575,#9576,#9577,#9578,#9579,#9580,#9581,
#9582,#9583,#9584,#9585,#9586,#9587,#9588,#9589,#9590,#9591,#9592,#9593,
#9594,#9595,#9596,#9597,#9598));
#9945=CLOSED_SHELL('',(#9599,#9600,#9601,#9602,#9603));
#9946=CLOSED_SHELL('',(#9604,#9605,#9606,#9607,#9608,#9609,#9610,#9611,
#9612,#9613,#9614,#9615,#9616,#9617,#9618,#9619,#9620,#9621));
#9947=CLOSED_SHELL('',(#9622,#9623,#9624,#9625,#9626,#9627));
#9948=CLOSED_SHELL('',(#9628,#9629,#9630,#9631,#9632,#9633));
#9949=CLOSED_SHELL('',(#9634));
#9950=CLOSED_SHELL('',(#9635));
#9951=CLOSED_SHELL('',(#9636,#9637,#9638,#9639,#9640,#9641,#9642,#9643,
#9644,#9645,#9646,#9647,#9648,#9649,#9650,#9651,#9652,#9653,#9654,#9655,
#9656,#9657,#9658,#9659,#9660,#9661,#9662,#9663,#9664,#9665,#9666,#9667,
#9668,#9669,#9670,#9671,#9672,#9673,#9674,#9675,#9676,#9677,#9678,#9679,
#9680,#9681,#9682,#9683));
#9952=CLOSED_SHELL('',(#9684,#9685,#9686,#9687,#9688,#9689,#9690,#9691));
#9953=CLOSED_SHELL('',(#9692,#9693,#9694,#9695,#9696,#9697,#9698,#9699,
#9700,#9701,#9702,#9703,#9704,#9705,#9706));
#9954=CLOSED_SHELL('',(#9707,#9708,#9709,#9710,#9711));
#9955=CLOSED_SHELL('',(#9712,#9713,#9714,#9715,#9716,#9717,#9718,#9719,
#9720,#9721,#9722,#9723));
#9956=CLOSED_SHELL('',(#9724,#9725,#9726,#9727,#9728,#9729,#9730,#9731,
#9732,#9733,#9734,#9735,#9736,#9737,#9738,#9739,#9740,#9741,#9742,#9743,
#9744,#9745,#9746,#9747,#9748,#9749,#9750,#9751,#9752,#9753,#9754,#9755));
#9957=CLOSED_SHELL('',(#9756,#9757,#9758));
#9958=CLOSED_SHELL('',(#9759,#9760,#9761));
#9959=CLOSED_SHELL('',(#9762,#9763,#9764,#9765));
#9960=CLOSED_SHELL('',(#9766,#9767,#9768,#9769,#9770,#9771,#9772,#9773,
#9774));
#9961=CLOSED_SHELL('',(#9775,#9776,#9777,#9778,#9779,#9780,#9781,#9782,
#9783,#9784,#9785,#9786,#9787,#9788,#9789,#9790,#9791,#9792,#9793,#9794,
#9795,#9796,#9797,#9798,#9799,#9800,#9801,#9802,#9803,#9804,#9805,#9806,
#9807,#9808,#9809,#9810,#9811,#9812,#9813,#9814,#9815,#9816,#9817,#9818,
#9819,#9820,#9821,#9822,#9823,#9824,#9825,#9826,#9827,#9828,#9829,#9830,
#9831,#9832,#9833,#9834,#9835,#9836,#9837,#9838,#9839,#9840,#9841,#9842,
#9843,#9844,#9845,#9846,#9847,#9848,#9849,#9850,#9851,#9852,#9853,#9854,
#9855));
#9962=CLOSED_SHELL('',(#9856,#9857,#9858,#9859,#9860,#9861,#9862,#9863,
#9864,#9865,#9866,#9867,#9868,#9869,#9870,#9871,#9872,#9873,#9874,#9875,
#9876,#9877,#9878,#9879,#9880,#9881,#9882,#9883,#9884,#9885,#9886,#9887));
#9963=CLOSED_SHELL('',(#9888,#9889,#9890,#9891,#9892,#9893));
#9964=CLOSED_SHELL('',(#9894,#9895,#9896,#9897,#9898,#9899,#9900,#9901,
#9902,#9903,#9904,#9905,#9906,#9907));
#9965=CLOSED_SHELL('',(#9908));
#9966=CLOSED_SHELL('',(#9909,#9910,#9911,#9912,#9913,#9914,#9915,#9916,
#9917,#9918,#9919));
#9967=CLOSED_SHELL('',(#9920));
#9968=CLOSED_SHELL('',(#9921,#9922,#9923,#9924,#9925,#9926,#9927,#9928,
#9929,#9930,#9931,#9932,#9933,#9934,#9935,#9936,#9937,#9938,#9939,#9940,
#9941));
#9969=DERIVED_UNIT_ELEMENT(#10023,1.);
#9970=DERIVED_UNIT_ELEMENT(#33018,-3.);
#9971=DERIVED_UNIT_ELEMENT(#10023,1.);
#9972=DERIVED_UNIT_ELEMENT(#33018,-3.);
#9973=DERIVED_UNIT_ELEMENT(#10023,1.);
#9974=DERIVED_UNIT_ELEMENT(#33018,-3.);
#9975=DERIVED_UNIT_ELEMENT(#10023,1.);
#9976=DERIVED_UNIT_ELEMENT(#33018,-3.);
#9977=DERIVED_UNIT_ELEMENT(#10023,1.);
#9978=DERIVED_UNIT_ELEMENT(#33018,-3.);
#9979=DERIVED_UNIT_ELEMENT(#10023,1.);
#9980=DERIVED_UNIT_ELEMENT(#33018,-3.);
#9981=DERIVED_UNIT_ELEMENT(#10023,1.);
#9982=DERIVED_UNIT_ELEMENT(#33018,-3.);
#9983=DERIVED_UNIT_ELEMENT(#10023,1.);
#9984=DERIVED_UNIT_ELEMENT(#33018,-3.);
#9985=DERIVED_UNIT_ELEMENT(#10023,1.);
#9986=DERIVED_UNIT_ELEMENT(#33018,-3.);
#9987=DERIVED_UNIT_ELEMENT(#10023,1.);
#9988=DERIVED_UNIT_ELEMENT(#33018,-3.);
#9989=DERIVED_UNIT_ELEMENT(#10023,1.);
#9990=DERIVED_UNIT_ELEMENT(#33018,-3.);
#9991=DERIVED_UNIT_ELEMENT(#10023,1.);
#9992=DERIVED_UNIT_ELEMENT(#33018,-3.);
#9993=DERIVED_UNIT_ELEMENT(#10023,1.);
#9994=DERIVED_UNIT_ELEMENT(#33018,-3.);
#9995=DERIVED_UNIT_ELEMENT(#10023,1.);
#9996=DERIVED_UNIT_ELEMENT(#33018,-3.);
#9997=DERIVED_UNIT_ELEMENT(#10023,1.);
#9998=DERIVED_UNIT_ELEMENT(#33018,-3.);
#9999=DERIVED_UNIT_ELEMENT(#10023,1.);
#10000=DERIVED_UNIT_ELEMENT(#33018,-3.);
#10001=DERIVED_UNIT_ELEMENT(#10023,1.);
#10002=DERIVED_UNIT_ELEMENT(#33018,-3.);
#10003=DERIVED_UNIT_ELEMENT(#10023,1.);
#10004=DERIVED_UNIT_ELEMENT(#33018,-3.);
#10005=DERIVED_UNIT_ELEMENT(#10023,1.);
#10006=DERIVED_UNIT_ELEMENT(#33018,-3.);
#10007=DERIVED_UNIT_ELEMENT(#10023,1.);
#10008=DERIVED_UNIT_ELEMENT(#33018,-3.);
#10009=DERIVED_UNIT_ELEMENT(#10023,1.);
#10010=DERIVED_UNIT_ELEMENT(#33018,-3.);
#10011=DERIVED_UNIT_ELEMENT(#10023,1.);
#10012=DERIVED_UNIT_ELEMENT(#33018,-3.);
#10013=DERIVED_UNIT_ELEMENT(#10023,1.);
#10014=DERIVED_UNIT_ELEMENT(#33018,-3.);
#10015=DERIVED_UNIT_ELEMENT(#10023,1.);
#10016=DERIVED_UNIT_ELEMENT(#33018,-3.);
#10017=DERIVED_UNIT_ELEMENT(#10023,1.);
#10018=DERIVED_UNIT_ELEMENT(#33018,-3.);
#10019=DERIVED_UNIT_ELEMENT(#10023,1.);
#10020=DERIVED_UNIT_ELEMENT(#33018,-3.);
#10021=DERIVED_UNIT_ELEMENT(#10023,1.);
#10022=DERIVED_UNIT_ELEMENT(#33018,-3.);
#10023=(
MASS_UNIT()
NAMED_UNIT(*)
SI_UNIT(.KILO.,.GRAM.)
);
#10024=DERIVED_UNIT((#9969,#9970));
#10025=DERIVED_UNIT((#9971,#9972));
#10026=DERIVED_UNIT((#9973,#9974));
#10027=DERIVED_UNIT((#9975,#9976));
#10028=DERIVED_UNIT((#9977,#9978));
#10029=DERIVED_UNIT((#9979,#9980));
#10030=DERIVED_UNIT((#9981,#9982));
#10031=DERIVED_UNIT((#9983,#9984));
#10032=DERIVED_UNIT((#9985,#9986));
#10033=DERIVED_UNIT((#9987,#9988));
#10034=DERIVED_UNIT((#9989,#9990));
#10035=DERIVED_UNIT((#9991,#9992));
#10036=DERIVED_UNIT((#9993,#9994));
#10037=DERIVED_UNIT((#9995,#9996));
#10038=DERIVED_UNIT((#9997,#9998));
#10039=DERIVED_UNIT((#9999,#10000));
#10040=DERIVED_UNIT((#10001,#10002));
#10041=DERIVED_UNIT((#10003,#10004));
#10042=DERIVED_UNIT((#10005,#10006));
#10043=DERIVED_UNIT((#10007,#10008));
#10044=DERIVED_UNIT((#10009,#10010));
#10045=DERIVED_UNIT((#10011,#10012));
#10046=DERIVED_UNIT((#10013,#10014));
#10047=DERIVED_UNIT((#10015,#10016));
#10048=DERIVED_UNIT((#10017,#10018));
#10049=DERIVED_UNIT((#10019,#10020));
#10050=DERIVED_UNIT((#10021,#10022));
#10051=MEASURE_REPRESENTATION_ITEM('density measure',
POSITIVE_RATIO_MEASURE(7850.),#10024);
#10052=MEASURE_REPRESENTATION_ITEM('density measure',
POSITIVE_RATIO_MEASURE(7850.),#10025);
#10053=MEASURE_REPRESENTATION_ITEM('density measure',
POSITIVE_RATIO_MEASURE(7850.),#10026);
#10054=MEASURE_REPRESENTATION_ITEM('density measure',
POSITIVE_RATIO_MEASURE(7850.),#10027);
#10055=MEASURE_REPRESENTATION_ITEM('density measure',
POSITIVE_RATIO_MEASURE(7850.),#10028);
#10056=MEASURE_REPRESENTATION_ITEM('density measure',
POSITIVE_RATIO_MEASURE(7850.),#10029);
#10057=MEASURE_REPRESENTATION_ITEM('density measure',
POSITIVE_RATIO_MEASURE(7850.),#10030);
#10058=MEASURE_REPRESENTATION_ITEM('density measure',
POSITIVE_RATIO_MEASURE(7850.),#10031);
#10059=MEASURE_REPRESENTATION_ITEM('density measure',
POSITIVE_RATIO_MEASURE(7850.),#10032);
#10060=MEASURE_REPRESENTATION_ITEM('density measure',
POSITIVE_RATIO_MEASURE(7850.),#10033);
#10061=MEASURE_REPRESENTATION_ITEM('density measure',
POSITIVE_RATIO_MEASURE(7850.),#10034);
#10062=MEASURE_REPRESENTATION_ITEM('density measure',
POSITIVE_RATIO_MEASURE(7850.),#10035);
#10063=MEASURE_REPRESENTATION_ITEM('density measure',
POSITIVE_RATIO_MEASURE(7850.),#10036);
#10064=MEASURE_REPRESENTATION_ITEM('density measure',
POSITIVE_RATIO_MEASURE(7850.),#10037);
#10065=MEASURE_REPRESENTATION_ITEM('density measure',
POSITIVE_RATIO_MEASURE(7850.),#10038);
#10066=MEASURE_REPRESENTATION_ITEM('density measure',
POSITIVE_RATIO_MEASURE(7850.),#10039);
#10067=MEASURE_REPRESENTATION_ITEM('density measure',
POSITIVE_RATIO_MEASURE(7850.),#10040);
#10068=MEASURE_REPRESENTATION_ITEM('density measure',
POSITIVE_RATIO_MEASURE(7850.),#10041);
#10069=MEASURE_REPRESENTATION_ITEM('density measure',
POSITIVE_RATIO_MEASURE(7850.),#10042);
#10070=MEASURE_REPRESENTATION_ITEM('density measure',
POSITIVE_RATIO_MEASURE(7850.),#10043);
#10071=MEASURE_REPRESENTATION_ITEM('density measure',
POSITIVE_RATIO_MEASURE(7850.),#10044);
#10072=MEASURE_REPRESENTATION_ITEM('density measure',
POSITIVE_RATIO_MEASURE(7850.),#10045);
#10073=MEASURE_REPRESENTATION_ITEM('density measure',
POSITIVE_RATIO_MEASURE(7850.),#10046);
#10074=MEASURE_REPRESENTATION_ITEM('density measure',
POSITIVE_RATIO_MEASURE(7850.),#10047);
#10075=MEASURE_REPRESENTATION_ITEM('density measure',
POSITIVE_RATIO_MEASURE(7850.),#10048);
#10076=MEASURE_REPRESENTATION_ITEM('density measure',
POSITIVE_RATIO_MEASURE(7850.),#10049);
#10077=MEASURE_REPRESENTATION_ITEM('density measure',
POSITIVE_RATIO_MEASURE(7850.),#10050);
#10078=PROPERTY_DEFINITION_REPRESENTATION(#10213,#10132);
#10079=PROPERTY_DEFINITION_REPRESENTATION(#10214,#10133);
#10080=PROPERTY_DEFINITION_REPRESENTATION(#10215,#10134);
#10081=PROPERTY_DEFINITION_REPRESENTATION(#10216,#10135);
#10082=PROPERTY_DEFINITION_REPRESENTATION(#10217,#10136);
#10083=PROPERTY_DEFINITION_REPRESENTATION(#10218,#10137);
#10084=PROPERTY_DEFINITION_REPRESENTATION(#10219,#10138);
#10085=PROPERTY_DEFINITION_REPRESENTATION(#10220,#10139);
#10086=PROPERTY_DEFINITION_REPRESENTATION(#10221,#10140);
#10087=PROPERTY_DEFINITION_REPRESENTATION(#10222,#10141);
#10088=PROPERTY_DEFINITION_REPRESENTATION(#10223,#10142);
#10089=PROPERTY_DEFINITION_REPRESENTATION(#10224,#10143);
#10090=PROPERTY_DEFINITION_REPRESENTATION(#10225,#10144);
#10091=PROPERTY_DEFINITION_REPRESENTATION(#10226,#10145);
#10092=PROPERTY_DEFINITION_REPRESENTATION(#10227,#10146);
#10093=PROPERTY_DEFINITION_REPRESENTATION(#10228,#10147);
#10094=PROPERTY_DEFINITION_REPRESENTATION(#10229,#10148);
#10095=PROPERTY_DEFINITION_REPRESENTATION(#10230,#10149);
#10096=PROPERTY_DEFINITION_REPRESENTATION(#10231,#10150);
#10097=PROPERTY_DEFINITION_REPRESENTATION(#10232,#10151);
#10098=PROPERTY_DEFINITION_REPRESENTATION(#10233,#10152);
#10099=PROPERTY_DEFINITION_REPRESENTATION(#10234,#10153);
#10100=PROPERTY_DEFINITION_REPRESENTATION(#10235,#10154);
#10101=PROPERTY_DEFINITION_REPRESENTATION(#10236,#10155);
#10102=PROPERTY_DEFINITION_REPRESENTATION(#10237,#10156);
#10103=PROPERTY_DEFINITION_REPRESENTATION(#10238,#10157);
#10104=PROPERTY_DEFINITION_REPRESENTATION(#10239,#10158);
#10105=PROPERTY_DEFINITION_REPRESENTATION(#10240,#10159);
#10106=PROPERTY_DEFINITION_REPRESENTATION(#10241,#10160);
#10107=PROPERTY_DEFINITION_REPRESENTATION(#10242,#10161);
#10108=PROPERTY_DEFINITION_REPRESENTATION(#10243,#10162);
#10109=PROPERTY_DEFINITION_REPRESENTATION(#10244,#10163);
#10110=PROPERTY_DEFINITION_REPRESENTATION(#10245,#10164);
#10111=PROPERTY_DEFINITION_REPRESENTATION(#10246,#10165);
#10112=PROPERTY_DEFINITION_REPRESENTATION(#10247,#10166);
#10113=PROPERTY_DEFINITION_REPRESENTATION(#10248,#10167);
#10114=PROPERTY_DEFINITION_REPRESENTATION(#10249,#10168);
#10115=PROPERTY_DEFINITION_REPRESENTATION(#10250,#10169);
#10116=PROPERTY_DEFINITION_REPRESENTATION(#10251,#10170);
#10117=PROPERTY_DEFINITION_REPRESENTATION(#10252,#10171);
#10118=PROPERTY_DEFINITION_REPRESENTATION(#10253,#10172);
#10119=PROPERTY_DEFINITION_REPRESENTATION(#10254,#10173);
#10120=PROPERTY_DEFINITION_REPRESENTATION(#10255,#10174);
#10121=PROPERTY_DEFINITION_REPRESENTATION(#10256,#10175);
#10122=PROPERTY_DEFINITION_REPRESENTATION(#10257,#10176);
#10123=PROPERTY_DEFINITION_REPRESENTATION(#10258,#10177);
#10124=PROPERTY_DEFINITION_REPRESENTATION(#10259,#10178);
#10125=PROPERTY_DEFINITION_REPRESENTATION(#10260,#10179);
#10126=PROPERTY_DEFINITION_REPRESENTATION(#10261,#10180);
#10127=PROPERTY_DEFINITION_REPRESENTATION(#10262,#10181);
#10128=PROPERTY_DEFINITION_REPRESENTATION(#10263,#10182);
#10129=PROPERTY_DEFINITION_REPRESENTATION(#10264,#10183);
#10130=PROPERTY_DEFINITION_REPRESENTATION(#10265,#10184);
#10131=PROPERTY_DEFINITION_REPRESENTATION(#10266,#10185);
#10132=REPRESENTATION('material name',(#10186),#32986);
#10133=REPRESENTATION('density',(#10051),#32986);
#10134=REPRESENTATION('material name',(#10187),#32988);
#10135=REPRESENTATION('density',(#10052),#32988);
#10136=REPRESENTATION('material name',(#10188),#32989);
#10137=REPRESENTATION('density',(#10053),#32989);
#10138=REPRESENTATION('material name',(#10189),#32990);
#10139=REPRESENTATION('density',(#10054),#32990);
#10140=REPRESENTATION('material name',(#10190),#32991);
#10141=REPRESENTATION('density',(#10055),#32991);
#10142=REPRESENTATION('material name',(#10191),#32992);
#10143=REPRESENTATION('density',(#10056),#32992);
#10144=REPRESENTATION('material name',(#10192),#32993);
#10145=REPRESENTATION('density',(#10057),#32993);
#10146=REPRESENTATION('material name',(#10193),#32994);
#10147=REPRESENTATION('density',(#10058),#32994);
#10148=REPRESENTATION('material name',(#10194),#32995);
#10149=REPRESENTATION('density',(#10059),#32995);
#10150=REPRESENTATION('material name',(#10195),#32997);
#10151=REPRESENTATION('density',(#10060),#32997);
#10152=REPRESENTATION('material name',(#10196),#32998);
#10153=REPRESENTATION('density',(#10061),#32998);
#10154=REPRESENTATION('material name',(#10197),#32999);
#10155=REPRESENTATION('density',(#10062),#32999);
#10156=REPRESENTATION('material name',(#10198),#33000);
#10157=REPRESENTATION('density',(#10063),#33000);
#10158=REPRESENTATION('material name',(#10199),#33001);
#10159=REPRESENTATION('density',(#10064),#33001);
#10160=REPRESENTATION('material name',(#10200),#33002);
#10161=REPRESENTATION('density',(#10065),#33002);
#10162=REPRESENTATION('material name',(#10201),#33003);
#10163=REPRESENTATION('density',(#10066),#33003);
#10164=REPRESENTATION('material name',(#10202),#33004);
#10165=REPRESENTATION('density',(#10067),#33004);
#10166=REPRESENTATION('material name',(#10203),#33005);
#10167=REPRESENTATION('density',(#10068),#33005);
#10168=REPRESENTATION('material name',(#10204),#33006);
#10169=REPRESENTATION('density',(#10069),#33006);
#10170=REPRESENTATION('material name',(#10205),#33008);
#10171=REPRESENTATION('density',(#10070),#33008);
#10172=REPRESENTATION('material name',(#10206),#33009);
#10173=REPRESENTATION('density',(#10071),#33009);
#10174=REPRESENTATION('material name',(#10207),#33010);
#10175=REPRESENTATION('density',(#10072),#33010);
#10176=REPRESENTATION('material name',(#10208),#33011);
#10177=REPRESENTATION('density',(#10073),#33011);
#10178=REPRESENTATION('material name',(#10209),#33012);
#10179=REPRESENTATION('density',(#10074),#33012);
#10180=REPRESENTATION('material name',(#10210),#33013);
#10181=REPRESENTATION('density',(#10075),#33013);
#10182=REPRESENTATION('material name',(#10211),#33014);
#10183=REPRESENTATION('density',(#10076),#33014);
#10184=REPRESENTATION('material name',(#10212),#33015);
#10185=REPRESENTATION('density',(#10077),#33015);
#10186=DESCRIPTIVE_REPRESENTATION_ITEM('Steel','Steel');
#10187=DESCRIPTIVE_REPRESENTATION_ITEM('Steel','Steel');
#10188=DESCRIPTIVE_REPRESENTATION_ITEM('Steel','Steel');
#10189=DESCRIPTIVE_REPRESENTATION_ITEM('Steel','Steel');
#10190=DESCRIPTIVE_REPRESENTATION_ITEM('Steel','Steel');
#10191=DESCRIPTIVE_REPRESENTATION_ITEM('Steel','Steel');
#10192=DESCRIPTIVE_REPRESENTATION_ITEM('Steel','Steel');
#10193=DESCRIPTIVE_REPRESENTATION_ITEM('Steel','Steel');
#10194=DESCRIPTIVE_REPRESENTATION_ITEM('Steel','Steel');
#10195=DESCRIPTIVE_REPRESENTATION_ITEM('Steel','Steel');
#10196=DESCRIPTIVE_REPRESENTATION_ITEM('Steel','Steel');
#10197=DESCRIPTIVE_REPRESENTATION_ITEM('Steel','Steel');
#10198=DESCRIPTIVE_REPRESENTATION_ITEM('Steel','Steel');
#10199=DESCRIPTIVE_REPRESENTATION_ITEM('Steel','Steel');
#10200=DESCRIPTIVE_REPRESENTATION_ITEM('Steel','Steel');
#10201=DESCRIPTIVE_REPRESENTATION_ITEM('Steel','Steel');
#10202=DESCRIPTIVE_REPRESENTATION_ITEM('Steel','Steel');
#10203=DESCRIPTIVE_REPRESENTATION_ITEM('Steel','Steel');
#10204=DESCRIPTIVE_REPRESENTATION_ITEM('Steel','Steel');
#10205=DESCRIPTIVE_REPRESENTATION_ITEM('Steel','Steel');
#10206=DESCRIPTIVE_REPRESENTATION_ITEM('Steel','Steel');
#10207=DESCRIPTIVE_REPRESENTATION_ITEM('Steel','Steel');
#10208=DESCRIPTIVE_REPRESENTATION_ITEM('Steel','Steel');
#10209=DESCRIPTIVE_REPRESENTATION_ITEM('Steel','Steel');
#10210=DESCRIPTIVE_REPRESENTATION_ITEM('Steel','Steel');
#10211=DESCRIPTIVE_REPRESENTATION_ITEM('Steel','Steel');
#10212=DESCRIPTIVE_REPRESENTATION_ITEM('Steel','Steel');
#10213=PROPERTY_DEFINITION('material property','material name',#33157);
#10214=PROPERTY_DEFINITION('material property','density of part',#33157);
#10215=PROPERTY_DEFINITION('material property','material name',#33159);
#10216=PROPERTY_DEFINITION('material property','density of part',#33159);
#10217=PROPERTY_DEFINITION('material property','material name',#33160);
#10218=PROPERTY_DEFINITION('material property','density of part',#33160);
#10219=PROPERTY_DEFINITION('material property','material name',#33161);
#10220=PROPERTY_DEFINITION('material property','density of part',#33161);
#10221=PROPERTY_DEFINITION('material property','material name',#33162);
#10222=PROPERTY_DEFINITION('material property','density of part',#33162);
#10223=PROPERTY_DEFINITION('material property','material name',#33163);
#10224=PROPERTY_DEFINITION('material property','density of part',#33163);
#10225=PROPERTY_DEFINITION('material property','material name',#33164);
#10226=PROPERTY_DEFINITION('material property','density of part',#33164);
#10227=PROPERTY_DEFINITION('material property','material name',#33165);
#10228=PROPERTY_DEFINITION('material property','density of part',#33165);
#10229=PROPERTY_DEFINITION('material property','material name',#33166);
#10230=PROPERTY_DEFINITION('material property','density of part',#33166);
#10231=PROPERTY_DEFINITION('material property','material name',#33168);
#10232=PROPERTY_DEFINITION('material property','density of part',#33168);
#10233=PROPERTY_DEFINITION('material property','material name',#33169);
#10234=PROPERTY_DEFINITION('material property','density of part',#33169);
#10235=PROPERTY_DEFINITION('material property','material name',#33170);
#10236=PROPERTY_DEFINITION('material property','density of part',#33170);
#10237=PROPERTY_DEFINITION('material property','material name',#33171);
#10238=PROPERTY_DEFINITION('material property','density of part',#33171);
#10239=PROPERTY_DEFINITION('material property','material name',#33172);
#10240=PROPERTY_DEFINITION('material property','density of part',#33172);
#10241=PROPERTY_DEFINITION('material property','material name',#33173);
#10242=PROPERTY_DEFINITION('material property','density of part',#33173);
#10243=PROPERTY_DEFINITION('material property','material name',#33174);
#10244=PROPERTY_DEFINITION('material property','density of part',#33174);
#10245=PROPERTY_DEFINITION('material property','material name',#33175);
#10246=PROPERTY_DEFINITION('material property','density of part',#33175);
#10247=PROPERTY_DEFINITION('material property','material name',#33176);
#10248=PROPERTY_DEFINITION('material property','density of part',#33176);
#10249=PROPERTY_DEFINITION('material property','material name',#33177);
#10250=PROPERTY_DEFINITION('material property','density of part',#33177);
#10251=PROPERTY_DEFINITION('material property','material name',#33179);
#10252=PROPERTY_DEFINITION('material property','density of part',#33179);
#10253=PROPERTY_DEFINITION('material property','material name',#33180);
#10254=PROPERTY_DEFINITION('material property','density of part',#33180);
#10255=PROPERTY_DEFINITION('material property','material name',#33181);
#10256=PROPERTY_DEFINITION('material property','density of part',#33181);
#10257=PROPERTY_DEFINITION('material property','material name',#33182);
#10258=PROPERTY_DEFINITION('material property','density of part',#33182);
#10259=PROPERTY_DEFINITION('material property','material name',#33183);
#10260=PROPERTY_DEFINITION('material property','density of part',#33183);
#10261=PROPERTY_DEFINITION('material property','material name',#33184);
#10262=PROPERTY_DEFINITION('material property','density of part',#33184);
#10263=PROPERTY_DEFINITION('material property','material name',#33185);
#10264=PROPERTY_DEFINITION('material property','density of part',#33185);
#10265=PROPERTY_DEFINITION('material property','material name',#33186);
#10266=PROPERTY_DEFINITION('material property','density of part',#33186);
#10267=AXIS2_PLACEMENT_3D('',#13915,#11233,#11234);
#10268=AXIS2_PLACEMENT_3D('',#13916,#11235,#11236);
#10269=AXIS2_PLACEMENT_3D('',#13917,#11237,#11238);
#10270=AXIS2_PLACEMENT_3D('',#13922,#11240,#11241);
#10271=AXIS2_PLACEMENT_3D('',#13925,#11243,#11244);
#10272=AXIS2_PLACEMENT_3D('',#13926,#11245,#11246);
#10273=AXIS2_PLACEMENT_3D('',#13931,#11248,#11249);
#10274=AXIS2_PLACEMENT_3D('',#13934,#11251,#11252);
#10275=AXIS2_PLACEMENT_3D('',#13935,#11253,#11254);
#10276=AXIS2_PLACEMENT_3D('',#13940,#11256,#11257);
#10277=AXIS2_PLACEMENT_3D('',#13943,#11259,#11260);
#10278=AXIS2_PLACEMENT_3D('',#13944,#11261,#11262);
#10279=AXIS2_PLACEMENT_3D('',#13949,#11264,#11265);
#10280=AXIS2_PLACEMENT_3D('',#13952,#11267,#11268);
#10281=AXIS2_PLACEMENT_3D('',#13953,#11269,#11270);
#10282=AXIS2_PLACEMENT_3D('',#13958,#11272,#11273);
#10283=AXIS2_PLACEMENT_3D('',#13961,#11275,#11276);
#10284=AXIS2_PLACEMENT_3D('',#13962,#11277,#11278);
#10285=AXIS2_PLACEMENT_3D('',#13967,#11280,#11281);
#10286=AXIS2_PLACEMENT_3D('',#13970,#11283,#11284);
#10287=AXIS2_PLACEMENT_3D('',#13971,#11285,#11286);
#10288=AXIS2_PLACEMENT_3D('',#13976,#11288,#11289);
#10289=AXIS2_PLACEMENT_3D('',#13979,#11291,#11292);
#10290=AXIS2_PLACEMENT_3D('',#13980,#11293,#11294);
#10291=AXIS2_PLACEMENT_3D('',#13985,#11296,#11297);
#10292=AXIS2_PLACEMENT_3D('',#13988,#11299,#11300);
#10293=AXIS2_PLACEMENT_3D('',#13989,#11301,#11302);
#10294=AXIS2_PLACEMENT_3D('',#13994,#11304,#11305);
#10295=AXIS2_PLACEMENT_3D('',#13997,#11307,#11308);
#10296=AXIS2_PLACEMENT_3D('',#13998,#11309,#11310);
#10297=AXIS2_PLACEMENT_3D('',#14003,#11312,#11313);
#10298=AXIS2_PLACEMENT_3D('',#14006,#11315,#11316);
#10299=AXIS2_PLACEMENT_3D('',#14007,#11317,#11318);
#10300=AXIS2_PLACEMENT_3D('',#14012,#11320,#11321);
#10301=AXIS2_PLACEMENT_3D('',#14015,#11323,#11324);
#10302=AXIS2_PLACEMENT_3D('',#14016,#11325,#11326);
#10303=AXIS2_PLACEMENT_3D('',#14021,#11328,#11329);
#10304=AXIS2_PLACEMENT_3D('',#14024,#11331,#11332);
#10305=AXIS2_PLACEMENT_3D('',#14025,#11333,#11334);
#10306=AXIS2_PLACEMENT_3D('',#14030,#11336,#11337);
#10307=AXIS2_PLACEMENT_3D('',#14033,#11339,#11340);
#10308=AXIS2_PLACEMENT_3D('',#14034,#11341,#11342);
#10309=AXIS2_PLACEMENT_3D('',#14039,#11344,#11345);
#10310=AXIS2_PLACEMENT_3D('',#14042,#11347,#11348);
#10311=AXIS2_PLACEMENT_3D('',#14043,#11349,#11350);
#10312=AXIS2_PLACEMENT_3D('',#14048,#11352,#11353);
#10313=AXIS2_PLACEMENT_3D('',#14051,#11355,#11356);
#10314=AXIS2_PLACEMENT_3D('',#14052,#11357,#11358);
#10315=AXIS2_PLACEMENT_3D('',#14057,#11360,#11361);
#10316=AXIS2_PLACEMENT_3D('',#14060,#11363,#11364);
#10317=AXIS2_PLACEMENT_3D('',#14061,#11365,#11366);
#10318=AXIS2_PLACEMENT_3D('',#14066,#11368,#11369);
#10319=AXIS2_PLACEMENT_3D('',#14069,#11371,#11372);
#10320=AXIS2_PLACEMENT_3D('',#14070,#11373,#11374);
#10321=AXIS2_PLACEMENT_3D('',#14075,#11376,#11377);
#10322=AXIS2_PLACEMENT_3D('',#14078,#11379,#11380);
#10323=AXIS2_PLACEMENT_3D('',#14079,#11381,#11382);
#10324=AXIS2_PLACEMENT_3D('',#14084,#11384,#11385);
#10325=AXIS2_PLACEMENT_3D('',#14087,#11387,#11388);
#10326=AXIS2_PLACEMENT_3D('',#14088,#11389,#11390);
#10327=AXIS2_PLACEMENT_3D('',#14093,#11392,#11393);
#10328=AXIS2_PLACEMENT_3D('',#14096,#11395,#11396);
#10329=AXIS2_PLACEMENT_3D('',#14097,#11397,#11398);
#10330=AXIS2_PLACEMENT_3D('',#14102,#11400,#11401);
#10331=AXIS2_PLACEMENT_3D('',#14105,#11403,#11404);
#10332=AXIS2_PLACEMENT_3D('',#14106,#11405,#11406);
#10333=AXIS2_PLACEMENT_3D('',#14111,#11408,#11409);
#10334=AXIS2_PLACEMENT_3D('',#14114,#11411,#11412);
#10335=AXIS2_PLACEMENT_3D('',#14115,#11413,#11414);
#10336=AXIS2_PLACEMENT_3D('',#14120,#11416,#11417);
#10337=AXIS2_PLACEMENT_3D('',#14123,#11419,#11420);
#10338=AXIS2_PLACEMENT_3D('',#14124,#11421,#11422);
#10339=AXIS2_PLACEMENT_3D('',#14129,#11424,#11425);
#10340=AXIS2_PLACEMENT_3D('',#14132,#11427,#11428);
#10341=AXIS2_PLACEMENT_3D('',#14133,#11429,#11430);
#10342=AXIS2_PLACEMENT_3D('',#14138,#11432,#11433);
#10343=AXIS2_PLACEMENT_3D('',#14141,#11435,#11436);
#10344=AXIS2_PLACEMENT_3D('',#14142,#11437,#11438);
#10345=AXIS2_PLACEMENT_3D('',#14147,#11440,#11441);
#10346=AXIS2_PLACEMENT_3D('',#14150,#11443,#11444);
#10347=AXIS2_PLACEMENT_3D('',#14151,#11445,#11446);
#10348=AXIS2_PLACEMENT_3D('',#14156,#11448,#11449);
#10349=AXIS2_PLACEMENT_3D('',#14159,#11451,#11452);
#10350=AXIS2_PLACEMENT_3D('',#14160,#11453,#11454);
#10351=AXIS2_PLACEMENT_3D('',#14165,#11456,#11457);
#10352=AXIS2_PLACEMENT_3D('',#14168,#11459,#11460);
#10353=AXIS2_PLACEMENT_3D('',#14169,#11461,#11462);
#10354=AXIS2_PLACEMENT_3D('',#14174,#11464,#11465);
#10355=AXIS2_PLACEMENT_3D('',#14177,#11467,#11468);
#10356=AXIS2_PLACEMENT_3D('',#14178,#11469,#11470);
#10357=AXIS2_PLACEMENT_3D('',#14183,#11472,#11473);
#10358=AXIS2_PLACEMENT_3D('',#14186,#11475,#11476);
#10359=AXIS2_PLACEMENT_3D('',#14187,#11477,#11478);
#10360=AXIS2_PLACEMENT_3D('',#14192,#11480,#11481);
#10361=AXIS2_PLACEMENT_3D('',#14195,#11483,#11484);
#10362=AXIS2_PLACEMENT_3D('',#14196,#11485,#11486);
#10363=AXIS2_PLACEMENT_3D('',#14201,#11488,#11489);
#10364=AXIS2_PLACEMENT_3D('',#14204,#11491,#11492);
#10365=AXIS2_PLACEMENT_3D('',#14205,#11493,#11494);
#10366=AXIS2_PLACEMENT_3D('',#14210,#11496,#11497);
#10367=AXIS2_PLACEMENT_3D('',#14213,#11499,#11500);
#10368=AXIS2_PLACEMENT_3D('',#14214,#11501,#11502);
#10369=AXIS2_PLACEMENT_3D('',#14219,#11504,#11505);
#10370=AXIS2_PLACEMENT_3D('',#14222,#11507,#11508);
#10371=AXIS2_PLACEMENT_3D('',#14223,#11509,#11510);
#10372=AXIS2_PLACEMENT_3D('',#14228,#11512,#11513);
#10373=AXIS2_PLACEMENT_3D('',#14231,#11515,#11516);
#10374=AXIS2_PLACEMENT_3D('',#14232,#11517,#11518);
#10375=AXIS2_PLACEMENT_3D('',#14237,#11520,#11521);
#10376=AXIS2_PLACEMENT_3D('',#14240,#11523,#11524);
#10377=AXIS2_PLACEMENT_3D('',#14241,#11525,#11526);
#10378=AXIS2_PLACEMENT_3D('',#14246,#11528,#11529);
#10379=AXIS2_PLACEMENT_3D('',#14249,#11531,#11532);
#10380=AXIS2_PLACEMENT_3D('',#14250,#11533,#11534);
#10381=AXIS2_PLACEMENT_3D('',#14255,#11536,#11537);
#10382=AXIS2_PLACEMENT_3D('',#14258,#11539,#11540);
#10383=AXIS2_PLACEMENT_3D('',#14259,#11541,#11542);
#10384=AXIS2_PLACEMENT_3D('',#14264,#11544,#11545);
#10385=AXIS2_PLACEMENT_3D('',#14267,#11547,#11548);
#10386=AXIS2_PLACEMENT_3D('',#14268,#11549,#11550);
#10387=AXIS2_PLACEMENT_3D('',#14273,#11552,#11553);
#10388=AXIS2_PLACEMENT_3D('',#14276,#11555,#11556);
#10389=AXIS2_PLACEMENT_3D('',#14277,#11557,#11558);
#10390=AXIS2_PLACEMENT_3D('',#14283,#11562,#11563);
#10391=AXIS2_PLACEMENT_3D('',#14286,#11566,#11567);
#10392=AXIS2_PLACEMENT_3D('',#14292,#11571,#11572);
#10393=AXIS2_PLACEMENT_3D('',#14295,#11575,#11576);
#10394=AXIS2_PLACEMENT_3D('',#14301,#11580,#11581);
#10395=AXIS2_PLACEMENT_3D('',#14304,#11584,#11585);
#10396=AXIS2_PLACEMENT_3D('',#14310,#11589,#11590);
#10397=AXIS2_PLACEMENT_3D('',#14313,#11593,#11594);
#10398=AXIS2_PLACEMENT_3D('',#14319,#11598,#11599);
#10399=AXIS2_PLACEMENT_3D('',#14322,#11602,#11603);
#10400=AXIS2_PLACEMENT_3D('',#14328,#11607,#11608);
#10401=AXIS2_PLACEMENT_3D('',#14331,#11611,#11612);
#10402=AXIS2_PLACEMENT_3D('',#14337,#11616,#11617);
#10403=AXIS2_PLACEMENT_3D('',#14340,#11620,#11621);
#10404=AXIS2_PLACEMENT_3D('',#14346,#11625,#11626);
#10405=AXIS2_PLACEMENT_3D('',#14349,#11629,#11630);
#10406=AXIS2_PLACEMENT_3D('',#14355,#11634,#11635);
#10407=AXIS2_PLACEMENT_3D('',#14358,#11638,#11639);
#10408=AXIS2_PLACEMENT_3D('',#14364,#11643,#11644);
#10409=AXIS2_PLACEMENT_3D('',#14367,#11647,#11648);
#10410=AXIS2_PLACEMENT_3D('',#14373,#11652,#11653);
#10411=AXIS2_PLACEMENT_3D('',#14376,#11656,#11657);
#10412=AXIS2_PLACEMENT_3D('',#14382,#11661,#11662);
#10413=AXIS2_PLACEMENT_3D('',#14385,#11665,#11666);
#10414=AXIS2_PLACEMENT_3D('',#14391,#11670,#11671);
#10415=AXIS2_PLACEMENT_3D('',#14394,#11674,#11675);
#10416=AXIS2_PLACEMENT_3D('',#14400,#11679,#11680);
#10417=AXIS2_PLACEMENT_3D('',#14403,#11683,#11684);
#10418=AXIS2_PLACEMENT_3D('',#14409,#11688,#11689);
#10419=AXIS2_PLACEMENT_3D('',#14412,#11692,#11693);
#10420=AXIS2_PLACEMENT_3D('',#14418,#11697,#11698);
#10421=AXIS2_PLACEMENT_3D('',#14421,#11701,#11702);
#10422=AXIS2_PLACEMENT_3D('',#14427,#11706,#11707);
#10423=AXIS2_PLACEMENT_3D('',#14430,#11710,#11711);
#10424=AXIS2_PLACEMENT_3D('',#14436,#11715,#11716);
#10425=AXIS2_PLACEMENT_3D('',#14439,#11719,#11720);
#10426=AXIS2_PLACEMENT_3D('',#14445,#11724,#11725);
#10427=AXIS2_PLACEMENT_3D('',#14448,#11728,#11729);
#10428=AXIS2_PLACEMENT_3D('',#14454,#11733,#11734);
#10429=AXIS2_PLACEMENT_3D('',#14457,#11737,#11738);
#10430=AXIS2_PLACEMENT_3D('',#14463,#11742,#11743);
#10431=AXIS2_PLACEMENT_3D('',#14466,#11746,#11747);
#10432=AXIS2_PLACEMENT_3D('',#14472,#11751,#11752);
#10433=AXIS2_PLACEMENT_3D('',#14475,#11755,#11756);
#10434=AXIS2_PLACEMENT_3D('',#14481,#11760,#11761);
#10435=AXIS2_PLACEMENT_3D('',#14484,#11764,#11765);
#10436=AXIS2_PLACEMENT_3D('',#14490,#11769,#11770);
#10437=AXIS2_PLACEMENT_3D('',#14493,#11773,#11774);
#10438=AXIS2_PLACEMENT_3D('',#14499,#11778,#11779);
#10439=AXIS2_PLACEMENT_3D('',#14502,#11782,#11783);
#10440=AXIS2_PLACEMENT_3D('',#14508,#11787,#11788);
#10441=AXIS2_PLACEMENT_3D('',#14511,#11791,#11792);
#10442=AXIS2_PLACEMENT_3D('',#14517,#11796,#11797);
#10443=AXIS2_PLACEMENT_3D('',#14520,#11800,#11801);
#10444=AXIS2_PLACEMENT_3D('',#14526,#11805,#11806);
#10445=AXIS2_PLACEMENT_3D('',#14529,#11809,#11810);
#10446=AXIS2_PLACEMENT_3D('',#14535,#11814,#11815);
#10447=AXIS2_PLACEMENT_3D('',#14538,#11818,#11819);
#10448=AXIS2_PLACEMENT_3D('',#14544,#11823,#11824);
#10449=AXIS2_PLACEMENT_3D('',#14547,#11827,#11828);
#10450=AXIS2_PLACEMENT_3D('',#14553,#11832,#11833);
#10451=AXIS2_PLACEMENT_3D('',#14556,#11836,#11837);
#10452=AXIS2_PLACEMENT_3D('',#14562,#11841,#11842);
#10453=AXIS2_PLACEMENT_3D('',#14565,#11845,#11846);
#10454=AXIS2_PLACEMENT_3D('',#14571,#11850,#11851);
#10455=AXIS2_PLACEMENT_3D('',#14574,#11854,#11855);
#10456=AXIS2_PLACEMENT_3D('',#14580,#11859,#11860);
#10457=AXIS2_PLACEMENT_3D('',#14583,#11863,#11864);
#10458=AXIS2_PLACEMENT_3D('',#14589,#11868,#11869);
#10459=AXIS2_PLACEMENT_3D('',#14592,#11872,#11873);
#10460=AXIS2_PLACEMENT_3D('',#14598,#11877,#11878);
#10461=AXIS2_PLACEMENT_3D('',#14601,#11881,#11882);
#10462=AXIS2_PLACEMENT_3D('',#14607,#11886,#11887);
#10463=AXIS2_PLACEMENT_3D('',#14610,#11890,#11891);
#10464=AXIS2_PLACEMENT_3D('',#14616,#11895,#11896);
#10465=AXIS2_PLACEMENT_3D('',#14619,#11899,#11900);
#10466=AXIS2_PLACEMENT_3D('',#14625,#11904,#11905);
#10467=AXIS2_PLACEMENT_3D('',#14628,#11908,#11909);
#10468=AXIS2_PLACEMENT_3D('',#14634,#11913,#11914);
#10469=AXIS2_PLACEMENT_3D('',#14637,#11917,#11918);
#10470=AXIS2_PLACEMENT_3D('',#14675,#11919,#11920);
#10471=AXIS2_PLACEMENT_3D('',#14711,#11921,#11922);
#10472=AXIS2_PLACEMENT_3D('',#14712,#11923,#11924);
#10473=AXIS2_PLACEMENT_3D('',#14869,#11925,#11926);
#10474=AXIS2_PLACEMENT_3D('',#14870,#11927,#11928);
#10475=AXIS2_PLACEMENT_3D('',#14873,#11929,#11930);
#10476=AXIS2_PLACEMENT_3D('',#15038,#11931,#11932);
#10477=AXIS2_PLACEMENT_3D('',#15039,#11933,#11934);
#10478=AXIS2_PLACEMENT_3D('',#15041,#11935,#11936);
#10479=AXIS2_PLACEMENT_3D('',#16163,#11938,#11939);
#10480=AXIS2_PLACEMENT_3D('',#16231,#11940,#11941);
#10481=AXIS2_PLACEMENT_3D('',#16232,#11942,#11943);
#10482=AXIS2_PLACEMENT_3D('',#16233,#11944,#11945);
#10483=AXIS2_PLACEMENT_3D('',#16491,#11946,#11947);
#10484=AXIS2_PLACEMENT_3D('',#16534,#11948,#11949);
#10485=AXIS2_PLACEMENT_3D('',#16536,#11950,#11951);
#10486=AXIS2_PLACEMENT_3D('',#16537,#11952,#11953);
#10487=AXIS2_PLACEMENT_3D('',#16670,#11954,#11955);
#10488=AXIS2_PLACEMENT_3D('',#16672,#11956,#11957);
#10489=AXIS2_PLACEMENT_3D('',#16674,#11959,#11960);
#10490=AXIS2_PLACEMENT_3D('',#16735,#11961,#11962);
#10491=AXIS2_PLACEMENT_3D('',#16748,#11963,#11964);
#10492=AXIS2_PLACEMENT_3D('',#16749,#11965,#11966);
#10493=AXIS2_PLACEMENT_3D('',#16750,#11967,#11968);
#10494=AXIS2_PLACEMENT_3D('',#16763,#11969,#11970);
#10495=AXIS2_PLACEMENT_3D('',#16896,#11971,#11972);
#10496=AXIS2_PLACEMENT_3D('',#16909,#11973,#11974);
#10497=AXIS2_PLACEMENT_3D('',#16910,#11975,#11976);
#10498=AXIS2_PLACEMENT_3D('',#16911,#11977,#11978);
#10499=AXIS2_PLACEMENT_3D('',#16924,#11979,#11980);
#10500=AXIS2_PLACEMENT_3D('',#16985,#11981,#11982);
#10501=AXIS2_PLACEMENT_3D('',#16987,#11983,#11984);
#10502=AXIS2_PLACEMENT_3D('',#16988,#11985,#11986);
#10503=AXIS2_PLACEMENT_3D('',#16990,#11987,#11988);
#10504=AXIS2_PLACEMENT_3D('',#16993,#11990,#11991);
#10505=AXIS2_PLACEMENT_3D('',#17022,#11992,#11993);
#10506=AXIS2_PLACEMENT_3D('',#17023,#11994,#11995);
#10507=AXIS2_PLACEMENT_3D('',#17626,#11996,#11997);
#10508=AXIS2_PLACEMENT_3D('',#17629,#11999,#12000);
#10509=AXIS2_PLACEMENT_3D('',#17630,#12001,#12002);
#10510=AXIS2_PLACEMENT_3D('',#17631,#12003,#12004);
#10511=AXIS2_PLACEMENT_3D('',#17632,#12005,#12006);
#10512=AXIS2_PLACEMENT_3D('',#17634,#12008,#12009);
#10513=AXIS2_PLACEMENT_3D('',#17643,#12014,#12015);
#10514=AXIS2_PLACEMENT_3D('',#17649,#12019,#12020);
#10515=AXIS2_PLACEMENT_3D('',#17653,#12023,#12024);
#10516=AXIS2_PLACEMENT_3D('',#17657,#12027,#12028);
#10517=AXIS2_PLACEMENT_3D('',#17659,#12030,#12031);
#10518=AXIS2_PLACEMENT_3D('',#17660,#12032,#12033);
#10519=AXIS2_PLACEMENT_3D('',#17661,#12034,#12035);
#10520=AXIS2_PLACEMENT_3D('',#17662,#12036,#12037);
#10521=AXIS2_PLACEMENT_3D('',#17673,#12041,#12042);
#10522=AXIS2_PLACEMENT_3D('',#17681,#12045,#12046);
#10523=AXIS2_PLACEMENT_3D('',#17689,#12049,#12050);
#10524=AXIS2_PLACEMENT_3D('',#17697,#12053,#12054);
#10525=AXIS2_PLACEMENT_3D('',#17709,#12057,#12058);
#10526=AXIS2_PLACEMENT_3D('',#17717,#12061,#12062);
#10527=AXIS2_PLACEMENT_3D('',#17726,#12065,#12066);
#10528=AXIS2_PLACEMENT_3D('',#17727,#12067,#12068);
#10529=AXIS2_PLACEMENT_3D('',#17732,#12070,#12071);
#10530=AXIS2_PLACEMENT_3D('',#17734,#12072,#12073);
#10531=AXIS2_PLACEMENT_3D('',#17741,#12077,#12078);
#10532=AXIS2_PLACEMENT_3D('',#17743,#12079,#12080);
#10533=AXIS2_PLACEMENT_3D('',#17746,#12082,#12083);
#10534=AXIS2_PLACEMENT_3D('',#17747,#12084,#12085);
#10535=AXIS2_PLACEMENT_3D('',#17749,#12086,#12087);
#10536=AXIS2_PLACEMENT_3D('',#17751,#12088,#12089);
#10537=AXIS2_PLACEMENT_3D('',#17752,#12090,#12091);
#10538=AXIS2_PLACEMENT_3D('',#17755,#12092,#12093);
#10539=AXIS2_PLACEMENT_3D('',#17757,#12095,#12096);
#10540=AXIS2_PLACEMENT_3D('',#17758,#12097,#12098);
#10541=AXIS2_PLACEMENT_3D('',#17760,#12099,#12100);
#10542=AXIS2_PLACEMENT_3D('',#17761,#12101,#12102);
#10543=AXIS2_PLACEMENT_3D('',#17763,#12103,#12104);
#10544=AXIS2_PLACEMENT_3D('',#17765,#12106,#12107);
#10545=AXIS2_PLACEMENT_3D('',#17767,#12108,#12109);
#10546=AXIS2_PLACEMENT_3D('',#17769,#12110,#12111);
#10547=AXIS2_PLACEMENT_3D('',#17770,#12112,#12113);
#10548=AXIS2_PLACEMENT_3D('',#17772,#12114,#12115);
#10549=AXIS2_PLACEMENT_3D('',#17774,#12116,#12117);
#10550=AXIS2_PLACEMENT_3D('',#17775,#12118,#12119);
#10551=AXIS2_PLACEMENT_3D('',#17777,#12120,#12121);
#10552=AXIS2_PLACEMENT_3D('',#17779,#12123,#12124);
#10553=AXIS2_PLACEMENT_3D('',#17780,#12125,#12126);
#10554=AXIS2_PLACEMENT_3D('',#17782,#12127,#12128);
#10555=AXIS2_PLACEMENT_3D('',#17783,#12129,#12130);
#10556=AXIS2_PLACEMENT_3D('',#17785,#12132,#12133);
#10557=AXIS2_PLACEMENT_3D('',#17787,#12134,#12135);
#10558=AXIS2_PLACEMENT_3D('',#17789,#12137,#12138);
#10559=AXIS2_PLACEMENT_3D('',#17791,#12139,#12140);
#10560=AXIS2_PLACEMENT_3D('',#17798,#12144,#12145);
#10561=AXIS2_PLACEMENT_3D('',#17800,#12146,#12147);
#10562=AXIS2_PLACEMENT_3D('',#17803,#12149,#12150);
#10563=AXIS2_PLACEMENT_3D('',#17804,#12151,#12152);
#10564=AXIS2_PLACEMENT_3D('',#17805,#12153,#12154);
#10565=AXIS2_PLACEMENT_3D('',#17809,#12157,#12158);
#10566=AXIS2_PLACEMENT_3D('',#17810,#12159,#12160);
#10567=AXIS2_PLACEMENT_3D('',#17812,#12162,#12163);
#10568=AXIS2_PLACEMENT_3D('',#17814,#12165,#12166);
#10569=AXIS2_PLACEMENT_3D('',#17815,#12167,#12168);
#10570=AXIS2_PLACEMENT_3D('',#17817,#12169,#12170);
#10571=AXIS2_PLACEMENT_3D('',#17818,#12171,#12172);
#10572=AXIS2_PLACEMENT_3D('',#17820,#12174,#12175);
#10573=AXIS2_PLACEMENT_3D('',#17822,#12176,#12177);
#10574=AXIS2_PLACEMENT_3D('',#17824,#12179,#12180);
#10575=AXIS2_PLACEMENT_3D('',#17825,#12181,#12182);
#10576=AXIS2_PLACEMENT_3D('',#17828,#12184,#12185);
#10577=AXIS2_PLACEMENT_3D('',#17829,#12186,#12187);
#10578=AXIS2_PLACEMENT_3D('',#17830,#12188,#12189);
#10579=AXIS2_PLACEMENT_3D('',#17832,#12191,#12192);
#10580=AXIS2_PLACEMENT_3D('',#17834,#12194,#12195);
#10581=AXIS2_PLACEMENT_3D('',#17835,#12196,#12197);
#10582=AXIS2_PLACEMENT_3D('',#17840,#12199,#12200);
#10583=AXIS2_PLACEMENT_3D('',#17843,#12202,#12203);
#10584=AXIS2_PLACEMENT_3D('',#17844,#12204,#12205);
#10585=AXIS2_PLACEMENT_3D('',#17847,#12206,#12207);
#10586=AXIS2_PLACEMENT_3D('',#17851,#12209,#12210);
#10587=AXIS2_PLACEMENT_3D('',#17853,#12212,#12213);
#10588=AXIS2_PLACEMENT_3D('',#17859,#12217,#12218);
#10589=AXIS2_PLACEMENT_3D('',#17865,#12222,#12223);
#10590=AXIS2_PLACEMENT_3D('',#17897,#12240,#12241);
#10591=AXIS2_PLACEMENT_3D('',#17898,#12242,#12243);
#10592=AXIS2_PLACEMENT_3D('',#17930,#12260,#12261);
#10593=AXIS2_PLACEMENT_3D('',#17931,#12262,#12263);
#10594=AXIS2_PLACEMENT_3D('',#17934,#12264,#12265);
#10595=AXIS2_PLACEMENT_3D('',#17937,#12267,#12268);
#10596=AXIS2_PLACEMENT_3D('',#17938,#12269,#12270);
#10597=AXIS2_PLACEMENT_3D('',#17939,#12271,#12272);
#10598=AXIS2_PLACEMENT_3D('',#17941,#12274,#12275);
#10599=AXIS2_PLACEMENT_3D('',#17943,#12277,#12278);
#10600=AXIS2_PLACEMENT_3D('',#17945,#12280,#12281);
#10601=AXIS2_PLACEMENT_3D('',#17947,#12283,#12284);
#10602=AXIS2_PLACEMENT_3D('',#17949,#12286,#12287);
#10603=AXIS2_PLACEMENT_3D('',#17951,#12289,#12290);
#10604=AXIS2_PLACEMENT_3D('',#17953,#12292,#12293);
#10605=AXIS2_PLACEMENT_3D('',#17954,#12294,#12295);
#10606=AXIS2_PLACEMENT_3D('',#17956,#12297,#12298);
#10607=AXIS2_PLACEMENT_3D('',#17958,#12300,#12301);
#10608=AXIS2_PLACEMENT_3D('',#17960,#12303,#12304);
#10609=AXIS2_PLACEMENT_3D('',#17962,#12306,#12307);
#10610=AXIS2_PLACEMENT_3D('',#17964,#12309,#12310);
#10611=AXIS2_PLACEMENT_3D('',#17966,#12312,#12313);
#10612=AXIS2_PLACEMENT_3D('',#17968,#12315,#12316);
#10613=AXIS2_PLACEMENT_3D('',#17969,#12317,#12318);
#10614=AXIS2_PLACEMENT_3D('',#17971,#12320,#12321);
#10615=AXIS2_PLACEMENT_3D('',#17973,#12323,#12324);
#10616=AXIS2_PLACEMENT_3D('',#17974,#12325,#12326);
#10617=AXIS2_PLACEMENT_3D('',#17977,#12327,#12328);
#10618=AXIS2_PLACEMENT_3D('',#17978,#12329,#12330);
#10619=AXIS2_PLACEMENT_3D('',#17981,#12332,#12333);
#10620=AXIS2_PLACEMENT_3D('',#17982,#12334,#12335);
#10621=AXIS2_PLACEMENT_3D('',#17984,#12336,#12337);
#10622=AXIS2_PLACEMENT_3D('',#17985,#12338,#12339);
#10623=AXIS2_PLACEMENT_3D('',#17987,#12340,#12341);
#10624=AXIS2_PLACEMENT_3D('',#17988,#12342,#12343);
#10625=AXIS2_PLACEMENT_3D('',#17990,#12345,#12346);
#10626=AXIS2_PLACEMENT_3D('',#17992,#12348,#12349);
#10627=AXIS2_PLACEMENT_3D('',#17993,#12350,#12351);
#10628=AXIS2_PLACEMENT_3D('',#17995,#12352,#12353);
#10629=AXIS2_PLACEMENT_3D('',#17996,#12354,#12355);
#10630=AXIS2_PLACEMENT_3D('',#17999,#12356,#12357);
#10631=AXIS2_PLACEMENT_3D('',#18002,#12359,#12360);
#10632=AXIS2_PLACEMENT_3D('',#18003,#12361,#12362);
#10633=AXIS2_PLACEMENT_3D('',#18042,#12363,#12364);
#10634=AXIS2_PLACEMENT_3D('',#18044,#12365,#12366);
#10635=AXIS2_PLACEMENT_3D('',#18045,#12367,#12368);
#10636=AXIS2_PLACEMENT_3D('',#18048,#12369,#12370);
#10637=AXIS2_PLACEMENT_3D('',#18051,#12372,#12373);
#10638=AXIS2_PLACEMENT_3D('',#18052,#12374,#12375);
#10639=AXIS2_PLACEMENT_3D('',#18053,#12376,#12377);
#10640=AXIS2_PLACEMENT_3D('',#18056,#12378,#12379);
#10641=AXIS2_PLACEMENT_3D('',#18058,#12380,#12381);
#10642=AXIS2_PLACEMENT_3D('',#18062,#12383,#12384);
#10643=AXIS2_PLACEMENT_3D('',#18064,#12385,#12386);
#10644=AXIS2_PLACEMENT_3D('',#18066,#12387,#12388);
#10645=AXIS2_PLACEMENT_3D('',#18069,#12390,#12391);
#10646=AXIS2_PLACEMENT_3D('',#18070,#12392,#12393);
#10647=AXIS2_PLACEMENT_3D('',#18073,#12394,#12395);
#10648=AXIS2_PLACEMENT_3D('',#18076,#12398,#12399);
#10649=AXIS2_PLACEMENT_3D('',#18082,#12403,#12404);
#10650=AXIS2_PLACEMENT_3D('',#18086,#12406,#12407);
#10651=AXIS2_PLACEMENT_3D('',#18088,#12409,#12410);
#10652=AXIS2_PLACEMENT_3D('',#18094,#12414,#12415);
#10653=AXIS2_PLACEMENT_3D('',#18095,#12416,#12417);
#10654=AXIS2_PLACEMENT_3D('',#18096,#12418,#12419);
#10655=AXIS2_PLACEMENT_3D('',#18097,#12420,#12421);
#10656=AXIS2_PLACEMENT_3D('',#18098,#12422,#12423);
#10657=AXIS2_PLACEMENT_3D('',#18099,#12424,#12425);
#10658=AXIS2_PLACEMENT_3D('',#18101,#12426,#12427);
#10659=AXIS2_PLACEMENT_3D('',#18103,#12429,#12430);
#10660=AXIS2_PLACEMENT_3D('',#18104,#12431,#12432);
#10661=AXIS2_PLACEMENT_3D('',#18106,#12434,#12435);
#10662=AXIS2_PLACEMENT_3D('',#18108,#12437,#12438);
#10663=AXIS2_PLACEMENT_3D('',#18109,#12439,#12440);
#10664=AXIS2_PLACEMENT_3D('',#18110,#12441,#12442);
#10665=AXIS2_PLACEMENT_3D('',#18111,#12443,#12444);
#10666=AXIS2_PLACEMENT_3D('',#18112,#12445,#12446);
#10667=AXIS2_PLACEMENT_3D('',#18407,#12447,#12448);
#10668=AXIS2_PLACEMENT_3D('',#18485,#12449,#12450);
#10669=AXIS2_PLACEMENT_3D('',#18852,#12451,#12452);
#10670=AXIS2_PLACEMENT_3D('',#18927,#12453,#12454);
#10671=AXIS2_PLACEMENT_3D('',#19221,#12455,#12456);
#10672=AXIS2_PLACEMENT_3D('',#19296,#12457,#12458);
#10673=AXIS2_PLACEMENT_3D('',#19589,#12459,#12460);
#10674=AXIS2_PLACEMENT_3D('',#19590,#12461,#12462);
#10675=AXIS2_PLACEMENT_3D('',#19591,#12463,#12464);
#10676=AXIS2_PLACEMENT_3D('',#19592,#12465,#12466);
#10677=AXIS2_PLACEMENT_3D('',#19593,#12467,#12468);
#10678=AXIS2_PLACEMENT_3D('',#19888,#12469,#12470);
#10679=AXIS2_PLACEMENT_3D('',#19966,#12471,#12472);
#10680=AXIS2_PLACEMENT_3D('',#20333,#12473,#12474);
#10681=AXIS2_PLACEMENT_3D('',#20408,#12475,#12476);
#10682=AXIS2_PLACEMENT_3D('',#20702,#12477,#12478);
#10683=AXIS2_PLACEMENT_3D('',#20777,#12479,#12480);
#10684=AXIS2_PLACEMENT_3D('',#21070,#12481,#12482);
#10685=AXIS2_PLACEMENT_3D('',#21071,#12483,#12484);
#10686=AXIS2_PLACEMENT_3D('',#21072,#12485,#12486);
#10687=AXIS2_PLACEMENT_3D('',#21073,#12487,#12488);
#10688=AXIS2_PLACEMENT_3D('',#21074,#12489,#12490);
#10689=AXIS2_PLACEMENT_3D('',#21075,#12491,#12492);
#10690=AXIS2_PLACEMENT_3D('',#21078,#12493,#12494);
#10691=AXIS2_PLACEMENT_3D('',#21079,#12495,#12496);
#10692=AXIS2_PLACEMENT_3D('',#21080,#12497,#12498);
#10693=AXIS2_PLACEMENT_3D('',#21081,#12499,#12500);
#10694=AXIS2_PLACEMENT_3D('',#21082,#12501,#12502);
#10695=AXIS2_PLACEMENT_3D('',#21083,#12503,#12504);
#10696=AXIS2_PLACEMENT_3D('',#21084,#12505,#12506);
#10697=AXIS2_PLACEMENT_3D('',#21085,#12507,#12508);
#10698=AXIS2_PLACEMENT_3D('',#21086,#12509,#12510);
#10699=AXIS2_PLACEMENT_3D('',#21087,#12511,#12512);
#10700=AXIS2_PLACEMENT_3D('',#21088,#12513,#12514);
#10701=AXIS2_PLACEMENT_3D('',#21090,#12515,#12516);
#10702=AXIS2_PLACEMENT_3D('',#21091,#12517,#12518);
#10703=AXIS2_PLACEMENT_3D('',#21092,#12519,#12520);
#10704=AXIS2_PLACEMENT_3D('',#21093,#12521,#12522);
#10705=AXIS2_PLACEMENT_3D('',#21094,#12523,#12524);
#10706=AXIS2_PLACEMENT_3D('',#21096,#12525,#12526);
#10707=AXIS2_PLACEMENT_3D('',#21139,#12530,#12531);
#10708=AXIS2_PLACEMENT_3D('',#21771,#12551,#12552);
#10709=AXIS2_PLACEMENT_3D('',#21773,#12553,#12554);
#10710=AXIS2_PLACEMENT_3D('',#21800,#12557,#12558);
#10711=AXIS2_PLACEMENT_3D('',#21860,#12559,#12560);
#10712=AXIS2_PLACEMENT_3D('',#21863,#12561,#12562);
#10713=AXIS2_PLACEMENT_3D('',#21864,#12563,#12564);
#10714=AXIS2_PLACEMENT_3D('',#21893,#12567,#12568);
#10715=AXIS2_PLACEMENT_3D('',#21959,#12569,#12570);
#10716=AXIS2_PLACEMENT_3D('',#21961,#12571,#12572);
#10717=AXIS2_PLACEMENT_3D('',#21963,#12573,#12574);
#10718=AXIS2_PLACEMENT_3D('',#21964,#12575,#12576);
#10719=AXIS2_PLACEMENT_3D('',#21966,#12577,#12578);
#10720=AXIS2_PLACEMENT_3D('',#21968,#12579,#12580);
#10721=AXIS2_PLACEMENT_3D('',#21969,#12581,#12582);
#10722=AXIS2_PLACEMENT_3D('',#21972,#12583,#12584);
#10723=AXIS2_PLACEMENT_3D('',#22023,#12588,#12589);
#10724=AXIS2_PLACEMENT_3D('',#22066,#12590,#12591);
#10725=AXIS2_PLACEMENT_3D('',#22145,#12592,#12593);
#10726=AXIS2_PLACEMENT_3D('',#22147,#12595,#12596);
#10727=AXIS2_PLACEMENT_3D('',#22149,#12598,#12599);
#10728=AXIS2_PLACEMENT_3D('',#22206,#12601,#12602);
#10729=AXIS2_PLACEMENT_3D('',#22261,#12604,#12605);
#10730=AXIS2_PLACEMENT_3D('',#22262,#12606,#12607);
#10731=AXIS2_PLACEMENT_3D('',#22263,#12608,#12609);
#10732=AXIS2_PLACEMENT_3D('',#22264,#12610,#12611);
#10733=AXIS2_PLACEMENT_3D('',#22293,#12612,#12613);
#10734=AXIS2_PLACEMENT_3D('',#22294,#12614,#12615);
#10735=AXIS2_PLACEMENT_3D('',#22295,#12616,#12617);
#10736=AXIS2_PLACEMENT_3D('',#22352,#12618,#12619);
#10737=AXIS2_PLACEMENT_3D('',#22353,#12620,#12621);
#10738=AXIS2_PLACEMENT_3D('',#22354,#12622,#12623);
#10739=AXIS2_PLACEMENT_3D('',#22411,#12624,#12625);
#10740=AXIS2_PLACEMENT_3D('',#22412,#12626,#12627);
#10741=AXIS2_PLACEMENT_3D('',#22413,#12628,#12629);
#10742=AXIS2_PLACEMENT_3D('',#22470,#12630,#12631);
#10743=AXIS2_PLACEMENT_3D('',#22471,#12632,#12633);
#10744=AXIS2_PLACEMENT_3D('',#22472,#12634,#12635);
#10745=AXIS2_PLACEMENT_3D('',#22529,#12636,#12637);
#10746=AXIS2_PLACEMENT_3D('',#22530,#12638,#12639);
#10747=AXIS2_PLACEMENT_3D('',#22531,#12640,#12641);
#10748=AXIS2_PLACEMENT_3D('',#22588,#12642,#12643);
#10749=AXIS2_PLACEMENT_3D('',#22589,#12644,#12645);
#10750=AXIS2_PLACEMENT_3D('',#22590,#12646,#12647);
#10751=AXIS2_PLACEMENT_3D('',#22647,#12648,#12649);
#10752=AXIS2_PLACEMENT_3D('',#22648,#12650,#12651);
#10753=AXIS2_PLACEMENT_3D('',#22649,#12652,#12653);
#10754=AXIS2_PLACEMENT_3D('',#22706,#12654,#12655);
#10755=AXIS2_PLACEMENT_3D('',#22707,#12656,#12657);
#10756=AXIS2_PLACEMENT_3D('',#22708,#12658,#12659);
#10757=AXIS2_PLACEMENT_3D('',#22765,#12660,#12661);
#10758=AXIS2_PLACEMENT_3D('',#22766,#12662,#12663);
#10759=AXIS2_PLACEMENT_3D('',#22767,#12664,#12665);
#10760=AXIS2_PLACEMENT_3D('',#22824,#12666,#12667);
#10761=AXIS2_PLACEMENT_3D('',#22825,#12668,#12669);
#10762=AXIS2_PLACEMENT_3D('',#22826,#12670,#12671);
#10763=AXIS2_PLACEMENT_3D('',#23767,#12672,#12673);
#10764=AXIS2_PLACEMENT_3D('',#23769,#12675,#12676);
#10765=AXIS2_PLACEMENT_3D('',#23771,#12678,#12679);
#10766=AXIS2_PLACEMENT_3D('',#23773,#12681,#12682);
#10767=AXIS2_PLACEMENT_3D('',#23775,#12684,#12685);
#10768=AXIS2_PLACEMENT_3D('',#23776,#12686,#12687);
#10769=AXIS2_PLACEMENT_3D('',#23778,#12688,#12689);
#10770=AXIS2_PLACEMENT_3D('',#23805,#12692,#12693);
#10771=AXIS2_PLACEMENT_3D('',#23865,#12694,#12695);
#10772=AXIS2_PLACEMENT_3D('',#23867,#12696,#12697);
#10773=AXIS2_PLACEMENT_3D('',#23868,#12698,#12699);
#10774=AXIS2_PLACEMENT_3D('',#23870,#12700,#12701);
#10775=AXIS2_PLACEMENT_3D('',#23871,#12702,#12703);
#10776=AXIS2_PLACEMENT_3D('',#23873,#12704,#12705);
#10777=AXIS2_PLACEMENT_3D('',#23875,#12707,#12708);
#10778=AXIS2_PLACEMENT_3D('',#23876,#12709,#12710);
#10779=AXIS2_PLACEMENT_3D('',#23878,#12711,#12712);
#10780=AXIS2_PLACEMENT_3D('',#23880,#12714,#12715);
#10781=AXIS2_PLACEMENT_3D('',#23881,#12716,#12717);
#10782=AXIS2_PLACEMENT_3D('',#23883,#12719,#12720);
#10783=AXIS2_PLACEMENT_3D('',#23884,#12721,#12722);
#10784=AXIS2_PLACEMENT_3D('',#23886,#12723,#12724);
#10785=AXIS2_PLACEMENT_3D('',#23888,#12725,#12726);
#10786=AXIS2_PLACEMENT_3D('',#23889,#12727,#12728);
#10787=AXIS2_PLACEMENT_3D('',#23892,#12730,#12731);
#10788=AXIS2_PLACEMENT_3D('',#23893,#12732,#12733);
#10789=AXIS2_PLACEMENT_3D('',#23895,#12734,#12735);
#10790=AXIS2_PLACEMENT_3D('',#23897,#12736,#12737);
#10791=AXIS2_PLACEMENT_3D('',#23898,#12738,#12739);
#10792=AXIS2_PLACEMENT_3D('',#23900,#12740,#12741);
#10793=AXIS2_PLACEMENT_3D('',#23901,#12742,#12743);
#10794=AXIS2_PLACEMENT_3D('',#23902,#12744,#12745);
#10795=AXIS2_PLACEMENT_3D('',#23903,#12746,#12747);
#10796=AXIS2_PLACEMENT_3D('',#23906,#12749,#12750);
#10797=AXIS2_PLACEMENT_3D('',#23907,#12751,#12752);
#10798=AXIS2_PLACEMENT_3D('',#23910,#12754,#12755);
#10799=AXIS2_PLACEMENT_3D('',#23911,#12756,#12757);
#10800=AXIS2_PLACEMENT_3D('',#23924,#12764,#12765);
#10801=AXIS2_PLACEMENT_3D('',#23930,#12769,#12770);
#10802=AXIS2_PLACEMENT_3D('',#23934,#12773,#12774);
#10803=AXIS2_PLACEMENT_3D('',#23938,#12777,#12778);
#10804=AXIS2_PLACEMENT_3D('',#23942,#12781,#12782);
#10805=AXIS2_PLACEMENT_3D('',#23946,#12785,#12786);
#10806=AXIS2_PLACEMENT_3D('',#23948,#12788,#12789);
#10807=AXIS2_PLACEMENT_3D('',#23949,#12790,#12791);
#10808=AXIS2_PLACEMENT_3D('',#23950,#12792,#12793);
#10809=AXIS2_PLACEMENT_3D('',#23953,#12794,#12795);
#10810=AXIS2_PLACEMENT_3D('',#23955,#12797,#12798);
#10811=AXIS2_PLACEMENT_3D('',#23959,#12800,#12801);
#10812=AXIS2_PLACEMENT_3D('',#27726,#12802,#12803);
#10813=AXIS2_PLACEMENT_3D('',#27727,#12804,#12805);
#10814=AXIS2_PLACEMENT_3D('',#27728,#12806,#12807);
#10815=AXIS2_PLACEMENT_3D('',#27729,#12808,#12809);
#10816=AXIS2_PLACEMENT_3D('',#27732,#12810,#12811);
#10817=AXIS2_PLACEMENT_3D('',#27733,#12812,#12813);
#10818=AXIS2_PLACEMENT_3D('',#27736,#12815,#12816);
#10819=AXIS2_PLACEMENT_3D('',#27737,#12817,#12818);
#10820=AXIS2_PLACEMENT_3D('',#27739,#12819,#12820);
#10821=AXIS2_PLACEMENT_3D('',#27740,#12821,#12822);
#10822=AXIS2_PLACEMENT_3D('',#27742,#12823,#12824);
#10823=AXIS2_PLACEMENT_3D('',#27744,#12825,#12826);
#10824=AXIS2_PLACEMENT_3D('',#27745,#12827,#12828);
#10825=AXIS2_PLACEMENT_3D('',#27748,#12830,#12831);
#10826=AXIS2_PLACEMENT_3D('',#27749,#12832,#12833);
#10827=AXIS2_PLACEMENT_3D('',#27758,#12838,#12839);
#10828=AXIS2_PLACEMENT_3D('',#27764,#12843,#12844);
#10829=AXIS2_PLACEMENT_3D('',#27768,#12847,#12848);
#10830=AXIS2_PLACEMENT_3D('',#27772,#12851,#12852);
#10831=AXIS2_PLACEMENT_3D('',#27774,#12854,#12855);
#10832=AXIS2_PLACEMENT_3D('',#27775,#12856,#12857);
#10833=AXIS2_PLACEMENT_3D('',#27776,#12858,#12859);
#10834=AXIS2_PLACEMENT_3D('',#27777,#12860,#12861);
#10835=AXIS2_PLACEMENT_3D('',#27778,#12862,#12863);
#10836=AXIS2_PLACEMENT_3D('',#27779,#12864,#12865);
#10837=AXIS2_PLACEMENT_3D('',#27812,#12882,#12883);
#10838=AXIS2_PLACEMENT_3D('',#27818,#12887,#12888);
#10839=AXIS2_PLACEMENT_3D('',#27822,#12891,#12892);
#10840=AXIS2_PLACEMENT_3D('',#27826,#12895,#12896);
#10841=AXIS2_PLACEMENT_3D('',#27828,#12898,#12899);
#10842=AXIS2_PLACEMENT_3D('',#27853,#12912,#12913);
#10843=AXIS2_PLACEMENT_3D('',#27859,#12917,#12918);
#10844=AXIS2_PLACEMENT_3D('',#27863,#12921,#12922);
#10845=AXIS2_PLACEMENT_3D('',#27867,#12925,#12926);
#10846=AXIS2_PLACEMENT_3D('',#27871,#12929,#12930);
#10847=AXIS2_PLACEMENT_3D('',#27875,#12933,#12934);
#10848=AXIS2_PLACEMENT_3D('',#27879,#12937,#12938);
#10849=AXIS2_PLACEMENT_3D('',#27883,#12941,#12942);
#10850=AXIS2_PLACEMENT_3D('',#27887,#12945,#12946);
#10851=AXIS2_PLACEMENT_3D('',#27891,#12949,#12950);
#10852=AXIS2_PLACEMENT_3D('',#27895,#12953,#12954);
#10853=AXIS2_PLACEMENT_3D('',#27899,#12957,#12958);
#10854=AXIS2_PLACEMENT_3D('',#27901,#12960,#12961);
#10855=AXIS2_PLACEMENT_3D('',#27902,#12962,#12963);
#10856=AXIS2_PLACEMENT_3D('',#27908,#12967,#12968);
#10857=AXIS2_PLACEMENT_3D('',#27912,#12971,#12972);
#10858=AXIS2_PLACEMENT_3D('',#27916,#12975,#12976);
#10859=AXIS2_PLACEMENT_3D('',#27920,#12979,#12980);
#10860=AXIS2_PLACEMENT_3D('',#27924,#12983,#12984);
#10861=AXIS2_PLACEMENT_3D('',#27928,#12987,#12988);
#10862=AXIS2_PLACEMENT_3D('',#27932,#12991,#12992);
#10863=AXIS2_PLACEMENT_3D('',#27936,#12995,#12996);
#10864=AXIS2_PLACEMENT_3D('',#27940,#12999,#13000);
#10865=AXIS2_PLACEMENT_3D('',#27944,#13003,#13004);
#10866=AXIS2_PLACEMENT_3D('',#27948,#13007,#13008);
#10867=AXIS2_PLACEMENT_3D('',#27950,#13010,#13011);
#10868=AXIS2_PLACEMENT_3D('',#27951,#13012,#13013);
#10869=AXIS2_PLACEMENT_3D('',#27952,#13014,#13015);
#10870=AXIS2_PLACEMENT_3D('',#27954,#13016,#13017);
#10871=AXIS2_PLACEMENT_3D('',#27956,#13018,#13019);
#10872=AXIS2_PLACEMENT_3D('',#27957,#13020,#13021);
#10873=AXIS2_PLACEMENT_3D('',#27958,#13022,#13023);
#10874=AXIS2_PLACEMENT_3D('',#27959,#13024,#13025);
#10875=AXIS2_PLACEMENT_3D('',#27960,#13026,#13027);
#10876=AXIS2_PLACEMENT_3D('',#27961,#13028,#13029);
#10877=AXIS2_PLACEMENT_3D('',#27963,#13030,#13031);
#10878=AXIS2_PLACEMENT_3D('',#27966,#13033,#13034);
#10879=AXIS2_PLACEMENT_3D('',#27967,#13035,#13036);
#10880=AXIS2_PLACEMENT_3D('',#27968,#13037,#13038);
#10881=AXIS2_PLACEMENT_3D('',#27969,#13039,#13040);
#10882=AXIS2_PLACEMENT_3D('',#27970,#13041,#13042);
#10883=AXIS2_PLACEMENT_3D('',#27972,#13043,#13044);
#10884=AXIS2_PLACEMENT_3D('',#27974,#13045,#13046);
#10885=AXIS2_PLACEMENT_3D('',#27975,#13047,#13048);
#10886=AXIS2_PLACEMENT_3D('',#27977,#13049,#13050);
#10887=AXIS2_PLACEMENT_3D('',#27979,#13051,#13052);
#10888=AXIS2_PLACEMENT_3D('',#27980,#13053,#13054);
#10889=AXIS2_PLACEMENT_3D('',#27982,#13056,#13057);
#10890=AXIS2_PLACEMENT_3D('',#27984,#13059,#13060);
#10891=AXIS2_PLACEMENT_3D('',#27985,#13061,#13062);
#10892=AXIS2_PLACEMENT_3D('',#27986,#13063,#13064);
#10893=AXIS2_PLACEMENT_3D('',#27987,#13065,#13066);
#10894=AXIS2_PLACEMENT_3D('',#27988,#13067,#13068);
#10895=AXIS2_PLACEMENT_3D('',#27989,#13069,#13070);
#10896=AXIS2_PLACEMENT_3D('',#27990,#13071,#13072);
#10897=AXIS2_PLACEMENT_3D('',#27991,#13073,#13074);
#10898=AXIS2_PLACEMENT_3D('',#27992,#13075,#13076);
#10899=AXIS2_PLACEMENT_3D('',#27993,#13077,#13078);
#10900=AXIS2_PLACEMENT_3D('',#27994,#13079,#13080);
#10901=AXIS2_PLACEMENT_3D('',#27995,#13081,#13082);
#10902=AXIS2_PLACEMENT_3D('',#27996,#13083,#13084);
#10903=AXIS2_PLACEMENT_3D('',#27997,#13085,#13086);
#10904=AXIS2_PLACEMENT_3D('',#27998,#13087,#13088);
#10905=AXIS2_PLACEMENT_3D('',#27999,#13089,#13090);
#10906=AXIS2_PLACEMENT_3D('',#28001,#13091,#13092);
#10907=AXIS2_PLACEMENT_3D('',#28004,#13094,#13095);
#10908=AXIS2_PLACEMENT_3D('',#28005,#13096,#13097);
#10909=AXIS2_PLACEMENT_3D('',#28007,#13098,#13099);
#10910=AXIS2_PLACEMENT_3D('',#28008,#13100,#13101);
#10911=AXIS2_PLACEMENT_3D('',#28011,#13103,#13104);
#10912=AXIS2_PLACEMENT_3D('',#28012,#13105,#13106);
#10913=AXIS2_PLACEMENT_3D('',#28013,#13107,#13108);
#10914=AXIS2_PLACEMENT_3D('',#28015,#13109,#13110);
#10915=AXIS2_PLACEMENT_3D('',#28017,#13111,#13112);
#10916=AXIS2_PLACEMENT_3D('',#28018,#13113,#13114);
#10917=AXIS2_PLACEMENT_3D('',#28021,#13116,#13117);
#10918=AXIS2_PLACEMENT_3D('',#28022,#13118,#13119);
#10919=AXIS2_PLACEMENT_3D('',#28023,#13120,#13121);
#10920=AXIS2_PLACEMENT_3D('',#28025,#13122,#13123);
#10921=AXIS2_PLACEMENT_3D('',#28026,#13124,#13125);
#10922=AXIS2_PLACEMENT_3D('',#28028,#13127,#13128);
#10923=AXIS2_PLACEMENT_3D('',#28029,#13129,#13130);
#10924=AXIS2_PLACEMENT_3D('',#28030,#13131,#13132);
#10925=AXIS2_PLACEMENT_3D('',#28033,#13133,#13134);
#10926=AXIS2_PLACEMENT_3D('',#28053,#13136,#13137);
#10927=AXIS2_PLACEMENT_3D('',#28069,#13139,#13140);
#10928=AXIS2_PLACEMENT_3D('',#28081,#13142,#13143);
#10929=AXIS2_PLACEMENT_3D('',#28101,#13145,#13146);
#10930=AXIS2_PLACEMENT_3D('',#28108,#13147,#13148);
#10931=AXIS2_PLACEMENT_3D('',#28120,#13150,#13151);
#10932=AXIS2_PLACEMENT_3D('',#28140,#13153,#13154);
#10933=AXIS2_PLACEMENT_3D('',#28147,#13155,#13156);
#10934=AXIS2_PLACEMENT_3D('',#28159,#13158,#13159);
#10935=AXIS2_PLACEMENT_3D('',#28179,#13161,#13162);
#10936=AXIS2_PLACEMENT_3D('',#28181,#13163,#13164);
#10937=AXIS2_PLACEMENT_3D('',#28188,#13165,#13166);
#10938=AXIS2_PLACEMENT_3D('',#28191,#13167,#13168);
#10939=AXIS2_PLACEMENT_3D('',#28211,#13170,#13171);
#10940=AXIS2_PLACEMENT_3D('',#28227,#13173,#13174);
#10941=AXIS2_PLACEMENT_3D('',#28239,#13176,#13177);
#10942=AXIS2_PLACEMENT_3D('',#28259,#13179,#13180);
#10943=AXIS2_PLACEMENT_3D('',#28266,#13181,#13182);
#10944=AXIS2_PLACEMENT_3D('',#28278,#13184,#13185);
#10945=AXIS2_PLACEMENT_3D('',#28298,#13187,#13188);
#10946=AXIS2_PLACEMENT_3D('',#28305,#13189,#13190);
#10947=AXIS2_PLACEMENT_3D('',#28317,#13192,#13193);
#10948=AXIS2_PLACEMENT_3D('',#28337,#13195,#13196);
#10949=AXIS2_PLACEMENT_3D('',#28344,#13197,#13198);
#10950=AXIS2_PLACEMENT_3D('',#28356,#13200,#13201);
#10951=AXIS2_PLACEMENT_3D('',#28376,#13203,#13204);
#10952=AXIS2_PLACEMENT_3D('',#28383,#13205,#13206);
#10953=AXIS2_PLACEMENT_3D('',#28384,#13207,#13208);
#10954=AXIS2_PLACEMENT_3D('',#28385,#13209,#13210);
#10955=AXIS2_PLACEMENT_3D('',#28386,#13211,#13212);
#10956=AXIS2_PLACEMENT_3D('',#28387,#13213,#13214);
#10957=AXIS2_PLACEMENT_3D('',#28388,#13215,#13216);
#10958=AXIS2_PLACEMENT_3D('',#28389,#13217,#13218);
#10959=AXIS2_PLACEMENT_3D('',#28390,#13219,#13220);
#10960=AXIS2_PLACEMENT_3D('',#28392,#13221,#13222);
#10961=AXIS2_PLACEMENT_3D('',#28394,#13223,#13224);
#10962=AXIS2_PLACEMENT_3D('',#28395,#13225,#13226);
#10963=AXIS2_PLACEMENT_3D('',#28396,#13227,#13228);
#10964=AXIS2_PLACEMENT_3D('',#28398,#13229,#13230);
#10965=AXIS2_PLACEMENT_3D('',#28399,#13231,#13232);
#10966=AXIS2_PLACEMENT_3D('',#28401,#13233,#13234);
#10967=AXIS2_PLACEMENT_3D('',#28404,#13236,#13237);
#10968=AXIS2_PLACEMENT_3D('',#28405,#13238,#13239);
#10969=AXIS2_PLACEMENT_3D('',#28407,#13240,#13241);
#10970=AXIS2_PLACEMENT_3D('',#28410,#13243,#13244);
#10971=AXIS2_PLACEMENT_3D('',#28411,#13245,#13246);
#10972=AXIS2_PLACEMENT_3D('',#28440,#13249,#13250);
#10973=AXIS2_PLACEMENT_3D('',#28447,#13251,#13252);
#10974=AXIS2_PLACEMENT_3D('',#28449,#13253,#13254);
#10975=AXIS2_PLACEMENT_3D('',#28451,#13255,#13256);
#10976=AXIS2_PLACEMENT_3D('',#28452,#13257,#13258);
#10977=AXIS2_PLACEMENT_3D('',#28455,#13259,#13260);
#10978=AXIS2_PLACEMENT_3D('',#28456,#13261,#13262);
#10979=AXIS2_PLACEMENT_3D('',#28458,#13264,#13265);
#10980=AXIS2_PLACEMENT_3D('',#28461,#13267,#13268);
#10981=AXIS2_PLACEMENT_3D('',#28653,#13269,#13270);
#10982=AXIS2_PLACEMENT_3D('',#28655,#13271,#13272);
#10983=AXIS2_PLACEMENT_3D('',#28656,#13273,#13274);
#10984=AXIS2_PLACEMENT_3D('',#28660,#13276,#13277);
#10985=AXIS2_PLACEMENT_3D('',#28661,#13278,#13279);
#10986=AXIS2_PLACEMENT_3D('',#28662,#13280,#13281);
#10987=AXIS2_PLACEMENT_3D('',#29256,#13283,#13284);
#10988=AXIS2_PLACEMENT_3D('',#29258,#13285,#13286);
#10989=AXIS2_PLACEMENT_3D('',#29259,#13287,#13288);
#10990=AXIS2_PLACEMENT_3D('',#29452,#13290,#13291);
#10991=AXIS2_PLACEMENT_3D('',#29454,#13293,#13294);
#10992=AXIS2_PLACEMENT_3D('',#29456,#13296,#13297);
#10993=AXIS2_PLACEMENT_3D('',#29458,#13299,#13300);
#10994=AXIS2_PLACEMENT_3D('',#29460,#13302,#13303);
#10995=AXIS2_PLACEMENT_3D('',#29462,#13305,#13306);
#10996=AXIS2_PLACEMENT_3D('',#29464,#13307,#13308);
#10997=AXIS2_PLACEMENT_3D('',#29466,#13310,#13311);
#10998=AXIS2_PLACEMENT_3D('',#29468,#13313,#13314);
#10999=AXIS2_PLACEMENT_3D('',#29470,#13315,#13316);
#11000=AXIS2_PLACEMENT_3D('',#29471,#13317,#13318);
#11001=AXIS2_PLACEMENT_3D('',#29474,#13320,#13321);
#11002=AXIS2_PLACEMENT_3D('',#29475,#13322,#13323);
#11003=AXIS2_PLACEMENT_3D('',#29476,#13324,#13325);
#11004=AXIS2_PLACEMENT_3D('',#29481,#13327,#13328);
#11005=AXIS2_PLACEMENT_3D('',#29502,#13330,#13331);
#11006=AXIS2_PLACEMENT_3D('',#29507,#13333,#13334);
#11007=AXIS2_PLACEMENT_3D('',#29592,#13336,#13337);
#11008=AXIS2_PLACEMENT_3D('',#29597,#13339,#13340);
#11009=AXIS2_PLACEMENT_3D('',#29618,#13342,#13343);
#11010=AXIS2_PLACEMENT_3D('',#29623,#13345,#13346);
#11011=AXIS2_PLACEMENT_3D('',#29711,#13348,#13349);
#11012=AXIS2_PLACEMENT_3D('',#29716,#13351,#13352);
#11013=AXIS2_PLACEMENT_3D('',#29801,#13354,#13355);
#11014=AXIS2_PLACEMENT_3D('',#29825,#13357,#13358);
#11015=AXIS2_PLACEMENT_3D('',#29827,#13360,#13361);
#11016=AXIS2_PLACEMENT_3D('',#29832,#13363,#13364);
#11017=AXIS2_PLACEMENT_3D('',#29917,#13366,#13367);
#11018=AXIS2_PLACEMENT_3D('',#29922,#13369,#13370);
#11019=AXIS2_PLACEMENT_3D('',#29943,#13372,#13373);
#11020=AXIS2_PLACEMENT_3D('',#29948,#13375,#13376);
#11021=AXIS2_PLACEMENT_3D('',#30036,#13378,#13379);
#11022=AXIS2_PLACEMENT_3D('',#30041,#13381,#13382);
#11023=AXIS2_PLACEMENT_3D('',#30208,#13384,#13385);
#11024=AXIS2_PLACEMENT_3D('',#30209,#13386,#13387);
#11025=AXIS2_PLACEMENT_3D('',#30218,#13388,#13389);
#11026=AXIS2_PLACEMENT_3D('',#30227,#13390,#13391);
#11027=AXIS2_PLACEMENT_3D('',#30310,#13392,#13393);
#11028=AXIS2_PLACEMENT_3D('',#30311,#13394,#13395);
#11029=AXIS2_PLACEMENT_3D('',#30320,#13396,#13397);
#11030=AXIS2_PLACEMENT_3D('',#30329,#13398,#13399);
#11031=AXIS2_PLACEMENT_3D('',#30416,#13400,#13401);
#11032=AXIS2_PLACEMENT_3D('',#30425,#13402,#13403);
#11033=AXIS2_PLACEMENT_3D('',#30434,#13404,#13405);
#11034=AXIS2_PLACEMENT_3D('',#30517,#13406,#13407);
#11035=AXIS2_PLACEMENT_3D('',#30518,#13408,#13409);
#11036=AXIS2_PLACEMENT_3D('',#30527,#13410,#13411);
#11037=AXIS2_PLACEMENT_3D('',#30536,#13412,#13413);
#11038=AXIS2_PLACEMENT_3D('',#30623,#13414,#13415);
#11039=AXIS2_PLACEMENT_3D('',#30632,#13416,#13417);
#11040=AXIS2_PLACEMENT_3D('',#30641,#13418,#13419);
#11041=AXIS2_PLACEMENT_3D('',#30724,#13420,#13421);
#11042=AXIS2_PLACEMENT_3D('',#30725,#13422,#13423);
#11043=AXIS2_PLACEMENT_3D('',#30734,#13424,#13425);
#11044=AXIS2_PLACEMENT_3D('',#30743,#13426,#13427);
#11045=AXIS2_PLACEMENT_3D('',#30826,#13428,#13429);
#11046=AXIS2_PLACEMENT_3D('',#30827,#13430,#13431);
#11047=AXIS2_PLACEMENT_3D('',#30836,#13432,#13433);
#11048=AXIS2_PLACEMENT_3D('',#30845,#13434,#13435);
#11049=AXIS2_PLACEMENT_3D('',#30932,#13436,#13437);
#11050=AXIS2_PLACEMENT_3D('',#30941,#13438,#13439);
#11051=AXIS2_PLACEMENT_3D('',#30950,#13440,#13441);
#11052=AXIS2_PLACEMENT_3D('',#31033,#13442,#13443);
#11053=AXIS2_PLACEMENT_3D('',#31034,#13444,#13445);
#11054=AXIS2_PLACEMENT_3D('',#31043,#13446,#13447);
#11055=AXIS2_PLACEMENT_3D('',#31052,#13448,#13449);
#11056=AXIS2_PLACEMENT_3D('',#31139,#13450,#13451);
#11057=AXIS2_PLACEMENT_3D('',#31148,#13452,#13453);
#11058=AXIS2_PLACEMENT_3D('',#31157,#13454,#13455);
#11059=AXIS2_PLACEMENT_3D('',#31158,#13456,#13457);
#11060=AXIS2_PLACEMENT_3D('',#31159,#13458,#13459);
#11061=AXIS2_PLACEMENT_3D('',#31161,#13460,#13461);
#11062=AXIS2_PLACEMENT_3D('',#31163,#13462,#13463);
#11063=AXIS2_PLACEMENT_3D('',#31164,#13464,#13465);
#11064=AXIS2_PLACEMENT_3D('',#31166,#13466,#13467);
#11065=AXIS2_PLACEMENT_3D('',#31215,#13492,#13493);
#11066=AXIS2_PLACEMENT_3D('',#31221,#13497,#13498);
#11067=AXIS2_PLACEMENT_3D('',#31227,#13502,#13503);
#11068=AXIS2_PLACEMENT_3D('',#31233,#13507,#13508);
#11069=AXIS2_PLACEMENT_3D('',#31239,#13512,#13513);
#11070=AXIS2_PLACEMENT_3D('',#31243,#13516,#13517);
#11071=AXIS2_PLACEMENT_3D('',#31249,#13521,#13522);
#11072=AXIS2_PLACEMENT_3D('',#31252,#13523,#13524);
#11073=AXIS2_PLACEMENT_3D('',#31253,#13525,#13526);
#11074=AXIS2_PLACEMENT_3D('',#31255,#13528,#13529);
#11075=AXIS2_PLACEMENT_3D('',#31258,#13530,#13531);
#11076=AXIS2_PLACEMENT_3D('',#31259,#13532,#13533);
#11077=AXIS2_PLACEMENT_3D('',#31262,#13535,#13536);
#11078=AXIS2_PLACEMENT_3D('',#31263,#13537,#13538);
#11079=AXIS2_PLACEMENT_3D('',#31296,#13557,#13558);
#11080=AXIS2_PLACEMENT_3D('',#31297,#13559,#13560);
#11081=AXIS2_PLACEMENT_3D('',#31299,#13562,#13563);
#11082=AXIS2_PLACEMENT_3D('',#31301,#13565,#13566);
#11083=AXIS2_PLACEMENT_3D('',#31304,#13569,#13570);
#11084=AXIS2_PLACEMENT_3D('',#31306,#13572,#13573);
#11085=AXIS2_PLACEMENT_3D('',#31308,#13575,#13576);
#11086=AXIS2_PLACEMENT_3D('',#31310,#13578,#13579);
#11087=AXIS2_PLACEMENT_3D('',#31312,#13581,#13582);
#11088=AXIS2_PLACEMENT_3D('',#31313,#13583,#13584);
#11089=AXIS2_PLACEMENT_3D('',#31315,#13586,#13587);
#11090=AXIS2_PLACEMENT_3D('',#31316,#13588,#13589);
#11091=AXIS2_PLACEMENT_3D('',#31318,#13591,#13592);
#11092=AXIS2_PLACEMENT_3D('',#31319,#13593,#13594);
#11093=AXIS2_PLACEMENT_3D('',#31321,#13596,#13597);
#11094=AXIS2_PLACEMENT_3D('',#31322,#13598,#13599);
#11095=AXIS2_PLACEMENT_3D('',#31324,#13601,#13602);
#11096=AXIS2_PLACEMENT_3D('',#31325,#13603,#13604);
#11097=AXIS2_PLACEMENT_3D('',#31327,#13606,#13607);
#11098=AXIS2_PLACEMENT_3D('',#31328,#13608,#13609);
#11099=AXIS2_PLACEMENT_3D('',#31330,#13611,#13612);
#11100=AXIS2_PLACEMENT_3D('',#31331,#13613,#13614);
#11101=AXIS2_PLACEMENT_3D('',#31332,#13615,#13616);
#11102=AXIS2_PLACEMENT_3D('',#31334,#13618,#13619);
#11103=AXIS2_PLACEMENT_3D('',#31597,#13620,#13621);
#11104=AXIS2_PLACEMENT_3D('',#31667,#13622,#13623);
#11105=AXIS2_PLACEMENT_3D('',#31994,#13624,#13625);
#11106=AXIS2_PLACEMENT_3D('',#32061,#13626,#13627);
#11107=AXIS2_PLACEMENT_3D('',#32323,#13628,#13629);
#11108=AXIS2_PLACEMENT_3D('',#32390,#13630,#13631);
#11109=AXIS2_PLACEMENT_3D('',#32651,#13632,#13633);
#11110=AXIS2_PLACEMENT_3D('',#32652,#13634,#13635);
#11111=AXIS2_PLACEMENT_3D('',#32653,#13636,#13637);
#11112=AXIS2_PLACEMENT_3D('',#32654,#13638,#13639);
#11113=AXIS2_PLACEMENT_3D('',#32655,#13640,#13641);
#11114=AXIS2_PLACEMENT_3D('',#32656,#13642,#13643);
#11115=AXIS2_PLACEMENT_3D('',#32658,#13644,#13645);
#11116=AXIS2_PLACEMENT_3D('',#32660,#13646,#13647);
#11117=AXIS2_PLACEMENT_3D('',#32661,#13648,#13649);
#11118=AXIS2_PLACEMENT_3D('',#32664,#13651,#13652);
#11119=AXIS2_PLACEMENT_3D('',#32665,#13653,#13654);
#11120=AXIS2_PLACEMENT_3D('',#32667,#13655,#13656);
#11121=AXIS2_PLACEMENT_3D('',#32668,#13657,#13658);
#11122=AXIS2_PLACEMENT_3D('',#32669,#13659,#13660);
#11123=AXIS2_PLACEMENT_3D('',#32672,#13662,#13663);
#11124=AXIS2_PLACEMENT_3D('',#32673,#13664,#13665);
#11125=AXIS2_PLACEMENT_3D('',#32675,#13666,#13667);
#11126=AXIS2_PLACEMENT_3D('',#32676,#13668,#13669);
#11127=AXIS2_PLACEMENT_3D('',#32679,#13671,#13672);
#11128=AXIS2_PLACEMENT_3D('',#32680,#13673,#13674);
#11129=AXIS2_PLACEMENT_3D('',#32682,#13675,#13676);
#11130=AXIS2_PLACEMENT_3D('',#32683,#13677,#13678);
#11131=AXIS2_PLACEMENT_3D('',#32687,#13680,#13681);
#11132=AXIS2_PLACEMENT_3D('',#32688,#13682,#13683);
#11133=AXIS2_PLACEMENT_3D('',#32689,#13684,#13685);
#11134=AXIS2_PLACEMENT_3D('',#32692,#13686,#13687);
#11135=AXIS2_PLACEMENT_3D('',#32693,#13688,#13689);
#11136=AXIS2_PLACEMENT_3D('',#32695,#13691,#13692);
#11137=AXIS2_PLACEMENT_3D('',#32699,#13694,#13695);
#11138=AXIS2_PLACEMENT_3D('',#32700,#13696,#13697);
#11139=AXIS2_PLACEMENT_3D('',#32701,#13698,#13699);
#11140=AXIS2_PLACEMENT_3D('',#32704,#13700,#13701);
#11141=AXIS2_PLACEMENT_3D('',#32705,#13702,#13703);
#11142=AXIS2_PLACEMENT_3D('',#32707,#13705,#13706);
#11143=AXIS2_PLACEMENT_3D('',#32710,#13708,#13709);
#11144=AXIS2_PLACEMENT_3D('',#32711,#13710,#13711);
#11145=AXIS2_PLACEMENT_3D('',#32713,#13712,#13713);
#11146=AXIS2_PLACEMENT_3D('',#32714,#13714,#13715);
#11147=AXIS2_PLACEMENT_3D('',#32716,#13717,#13718);
#11148=AXIS2_PLACEMENT_3D('',#32717,#13719,#13720);
#11149=AXIS2_PLACEMENT_3D('',#32720,#13721,#13722);
#11150=AXIS2_PLACEMENT_3D('',#32721,#13723,#13724);
#11151=AXIS2_PLACEMENT_3D('',#32722,#13725,#13726);
#11152=AXIS2_PLACEMENT_3D('',#32723,#13727,#13728);
#11153=AXIS2_PLACEMENT_3D('',#32724,#13729,#13730);
#11154=AXIS2_PLACEMENT_3D('',#32725,#13731,#13732);
#11155=AXIS2_PLACEMENT_3D('',#32726,#13733,#13734);
#11156=AXIS2_PLACEMENT_3D('',#32727,#13735,#13736);
#11157=AXIS2_PLACEMENT_3D('',#32728,#13737,#13738);
#11158=AXIS2_PLACEMENT_3D('',#32729,#13739,#13740);
#11159=AXIS2_PLACEMENT_3D('',#32730,#13741,#13742);
#11160=AXIS2_PLACEMENT_3D('',#32731,#13743,#13744);
#11161=AXIS2_PLACEMENT_3D('',#32733,#13745,#13746);
#11162=AXIS2_PLACEMENT_3D('',#32734,#13747,#13748);
#11163=AXIS2_PLACEMENT_3D('',#32736,#13749,#13750);
#11164=AXIS2_PLACEMENT_3D('',#32738,#13752,#13753);
#11165=AXIS2_PLACEMENT_3D('',#32741,#13754,#13755);
#11166=AXIS2_PLACEMENT_3D('',#32742,#13756,#13757);
#11167=AXIS2_PLACEMENT_3D('',#32744,#13759,#13760);
#11168=AXIS2_PLACEMENT_3D('',#32746,#13761,#13762);
#11169=AXIS2_PLACEMENT_3D('',#32748,#13763,#13764);
#11170=AXIS2_PLACEMENT_3D('',#32749,#13765,#13766);
#11171=AXIS2_PLACEMENT_3D('',#32752,#13767,#13768);
#11172=AXIS2_PLACEMENT_3D('',#32753,#13769,#13770);
#11173=AXIS2_PLACEMENT_3D('',#32755,#13772,#13773);
#11174=AXIS2_PLACEMENT_3D('',#32757,#13775,#13776);
#11175=AXIS2_PLACEMENT_3D('',#32760,#13778,#13779);
#11176=AXIS2_PLACEMENT_3D('',#32761,#13780,#13781);
#11177=AXIS2_PLACEMENT_3D('',#32763,#13782,#13783);
#11178=AXIS2_PLACEMENT_3D('',#32764,#13784,#13785);
#11179=AXIS2_PLACEMENT_3D('',#32767,#13787,#13788);
#11180=AXIS2_PLACEMENT_3D('',#32768,#13789,#13790);
#11181=AXIS2_PLACEMENT_3D('',#32771,#13792,#13793);
#11182=AXIS2_PLACEMENT_3D('',#32772,#13794,#13795);
#11183=AXIS2_PLACEMENT_3D('',#32773,#13796,#13797);
#11184=AXIS2_PLACEMENT_3D('',#32774,#13798,#13799);
#11185=AXIS2_PLACEMENT_3D('',#32776,#13800,#13801);
#11186=AXIS2_PLACEMENT_3D('',#32777,#13802,#13803);
#11187=AXIS2_PLACEMENT_3D('',#32778,#13804,#13805);
#11188=AXIS2_PLACEMENT_3D('',#32779,#13806,#13807);
#11189=AXIS2_PLACEMENT_3D('',#32784,#13809,#13810);
#11190=AXIS2_PLACEMENT_3D('',#32788,#13812,#13813);
#11191=AXIS2_PLACEMENT_3D('',#32792,#13815,#13816);
#11192=AXIS2_PLACEMENT_3D('',#32796,#13818,#13819);
#11193=AXIS2_PLACEMENT_3D('',#32800,#13821,#13822);
#11194=AXIS2_PLACEMENT_3D('',#32803,#13824,#13825);
#11195=AXIS2_PLACEMENT_3D('',#32805,#13826,#13827);
#11196=AXIS2_PLACEMENT_3D('',#32806,#13828,#13829);
#11197=AXIS2_PLACEMENT_3D('',#32809,#13830,#13831);
#11198=AXIS2_PLACEMENT_3D('',#32813,#13833,#13834);
#11199=AXIS2_PLACEMENT_3D('',#32817,#13836,#13837);
#11200=AXIS2_PLACEMENT_3D('',#32821,#13839,#13840);
#11201=AXIS2_PLACEMENT_3D('',#32825,#13842,#13843);
#11202=AXIS2_PLACEMENT_3D('',#32829,#13845,#13846);
#11203=AXIS2_PLACEMENT_3D('',#32832,#13848,#13849);
#11204=AXIS2_PLACEMENT_3D('',#32833,#13850,#13851);
#11205=AXIS2_PLACEMENT_3D('',#32852,#13854,#13855);
#11206=AXIS2_PLACEMENT_3D('',#32868,#13857,#13858);
#11207=AXIS2_PLACEMENT_3D('',#32884,#13860,#13861);
#11208=AXIS2_PLACEMENT_3D('',#32900,#13863,#13864);
#11209=AXIS2_PLACEMENT_3D('',#32916,#13866,#13867);
#11210=AXIS2_PLACEMENT_3D('',#32929,#13868,#13869);
#11211=AXIS2_PLACEMENT_3D('',#32930,#13870,#13871);
#11212=AXIS2_PLACEMENT_3D('',#32931,#13872,#13873);
#11213=AXIS2_PLACEMENT_3D('',#32932,#13874,#13875);
#11214=AXIS2_PLACEMENT_3D('',#32933,#13876,#13877);
#11215=AXIS2_PLACEMENT_3D('',#32934,#13878,#13879);
#11216=AXIS2_PLACEMENT_3D('',#32935,#13880,#13881);
#11217=AXIS2_PLACEMENT_3D('',#32936,#13882,#13883);
#11218=AXIS2_PLACEMENT_3D('',#32937,#13884,#13885);
#11219=AXIS2_PLACEMENT_3D('',#32938,#13886,#13887);
#11220=AXIS2_PLACEMENT_3D('',#32939,#13888,#13889);
#11221=AXIS2_PLACEMENT_3D('',#32940,#13890,#13891);
#11222=AXIS2_PLACEMENT_3D('',#32941,#13892,#13893);
#11223=AXIS2_PLACEMENT_3D('',#32943,#13895,#13896);
#11224=AXIS2_PLACEMENT_3D('',#32944,#13897,#13898);
#11225=AXIS2_PLACEMENT_3D('',#32945,#13899,#13900);
#11226=AXIS2_PLACEMENT_3D('',#32946,#13901,#13902);
#11227=AXIS2_PLACEMENT_3D('',#32947,#13903,#13904);
#11228=AXIS2_PLACEMENT_3D('',#32948,#13905,#13906);
#11229=AXIS2_PLACEMENT_3D('',#32949,#13907,#13908);
#11230=AXIS2_PLACEMENT_3D('',#32950,#13909,#13910);
#11231=AXIS2_PLACEMENT_3D('',#32951,#13911,#13912);
#11232=AXIS2_PLACEMENT_3D('',#32952,#13913,#13914);
#11233=DIRECTION('axis',(0.,0.,1.));
#11234=DIRECTION('refdir',(1.,0.,0.));
#11235=DIRECTION('axis',(0.,0.,1.));
#11236=DIRECTION('refdir',(1.,0.,0.));
#11237=DIRECTION('center_axis',(0.,-1.,0.));
#11238=DIRECTION('ref_axis',(0.,0.,-1.));
#11239=DIRECTION('',(0.,-1.,0.));
#11240=DIRECTION('center_axis',(0.,-1.,0.));
#11241=DIRECTION('ref_axis',(0.,0.,-1.));
#11242=DIRECTION('',(0.,-1.,0.));
#11243=DIRECTION('center_axis',(0.,1.,0.));
#11244=DIRECTION('ref_axis',(0.,0.,1.));
#11245=DIRECTION('center_axis',(0.,-1.,0.));
#11246=DIRECTION('ref_axis',(0.,0.,-1.));
#11247=DIRECTION('',(0.,-1.,0.));
#11248=DIRECTION('center_axis',(0.,-1.,0.));
#11249=DIRECTION('ref_axis',(0.,0.,-1.));
#11250=DIRECTION('',(0.,-1.,0.));
#11251=DIRECTION('center_axis',(0.,1.,0.));
#11252=DIRECTION('ref_axis',(0.,0.,1.));
#11253=DIRECTION('center_axis',(0.,-1.,0.));
#11254=DIRECTION('ref_axis',(0.,0.,-1.));
#11255=DIRECTION('',(0.,-1.,0.));
#11256=DIRECTION('center_axis',(0.,-1.,0.));
#11257=DIRECTION('ref_axis',(0.,0.,-1.));
#11258=DIRECTION('',(0.,-1.,0.));
#11259=DIRECTION('center_axis',(0.,1.,0.));
#11260=DIRECTION('ref_axis',(0.,0.,1.));
#11261=DIRECTION('center_axis',(0.,-1.,0.));
#11262=DIRECTION('ref_axis',(0.,0.,-1.));
#11263=DIRECTION('',(0.,-1.,0.));
#11264=DIRECTION('center_axis',(0.,-1.,0.));
#11265=DIRECTION('ref_axis',(0.,0.,-1.));
#11266=DIRECTION('',(0.,-1.,0.));
#11267=DIRECTION('center_axis',(0.,1.,0.));
#11268=DIRECTION('ref_axis',(0.,0.,1.));
#11269=DIRECTION('center_axis',(0.,-1.,0.));
#11270=DIRECTION('ref_axis',(0.,0.,-1.));
#11271=DIRECTION('',(0.,-1.,0.));
#11272=DIRECTION('center_axis',(0.,-1.,0.));
#11273=DIRECTION('ref_axis',(0.,0.,-1.));
#11274=DIRECTION('',(0.,-1.,0.));
#11275=DIRECTION('center_axis',(0.,1.,0.));
#11276=DIRECTION('ref_axis',(0.,0.,1.));
#11277=DIRECTION('center_axis',(0.,-1.,0.));
#11278=DIRECTION('ref_axis',(0.,0.,-1.));
#11279=DIRECTION('',(0.,-1.,0.));
#11280=DIRECTION('center_axis',(0.,-1.,0.));
#11281=DIRECTION('ref_axis',(0.,0.,-1.));
#11282=DIRECTION('',(0.,-1.,0.));
#11283=DIRECTION('center_axis',(0.,1.,0.));
#11284=DIRECTION('ref_axis',(0.,0.,1.));
#11285=DIRECTION('center_axis',(0.,-1.,0.));
#11286=DIRECTION('ref_axis',(0.,0.,-1.));
#11287=DIRECTION('',(0.,-1.,0.));
#11288=DIRECTION('center_axis',(0.,-1.,0.));
#11289=DIRECTION('ref_axis',(0.,0.,-1.));
#11290=DIRECTION('',(0.,-1.,0.));
#11291=DIRECTION('center_axis',(0.,1.,0.));
#11292=DIRECTION('ref_axis',(0.,0.,1.));
#11293=DIRECTION('center_axis',(0.,-1.,0.));
#11294=DIRECTION('ref_axis',(0.,0.,-1.));
#11295=DIRECTION('',(0.,-1.,0.));
#11296=DIRECTION('center_axis',(0.,-1.,0.));
#11297=DIRECTION('ref_axis',(0.,0.,-1.));
#11298=DIRECTION('',(0.,-1.,0.));
#11299=DIRECTION('center_axis',(0.,1.,0.));
#11300=DIRECTION('ref_axis',(0.,0.,1.));
#11301=DIRECTION('center_axis',(0.,-1.,0.));
#11302=DIRECTION('ref_axis',(0.,0.,-1.));
#11303=DIRECTION('',(0.,-1.,0.));
#11304=DIRECTION('center_axis',(0.,-1.,0.));
#11305=DIRECTION('ref_axis',(0.,0.,-1.));
#11306=DIRECTION('',(0.,-1.,0.));
#11307=DIRECTION('center_axis',(0.,1.,0.));
#11308=DIRECTION('ref_axis',(0.,0.,1.));
#11309=DIRECTION('center_axis',(0.,-1.,0.));
#11310=DIRECTION('ref_axis',(0.,0.,-1.));
#11311=DIRECTION('',(0.,-1.,0.));
#11312=DIRECTION('center_axis',(0.,-1.,0.));
#11313=DIRECTION('ref_axis',(0.,0.,-1.));
#11314=DIRECTION('',(0.,-1.,0.));
#11315=DIRECTION('center_axis',(0.,1.,0.));
#11316=DIRECTION('ref_axis',(0.,0.,1.));
#11317=DIRECTION('center_axis',(0.,-1.,0.));
#11318=DIRECTION('ref_axis',(0.,0.,-1.));
#11319=DIRECTION('',(0.,-1.,0.));
#11320=DIRECTION('center_axis',(0.,-1.,0.));
#11321=DIRECTION('ref_axis',(0.,0.,-1.));
#11322=DIRECTION('',(0.,-1.,0.));
#11323=DIRECTION('center_axis',(0.,1.,0.));
#11324=DIRECTION('ref_axis',(0.,0.,1.));
#11325=DIRECTION('center_axis',(0.,-1.,0.));
#11326=DIRECTION('ref_axis',(0.,0.,-1.));
#11327=DIRECTION('',(0.,-1.,0.));
#11328=DIRECTION('center_axis',(0.,-1.,0.));
#11329=DIRECTION('ref_axis',(0.,0.,-1.));
#11330=DIRECTION('',(0.,-1.,0.));
#11331=DIRECTION('center_axis',(0.,1.,0.));
#11332=DIRECTION('ref_axis',(0.,0.,1.));
#11333=DIRECTION('center_axis',(0.,-1.,0.));
#11334=DIRECTION('ref_axis',(0.,0.,-1.));
#11335=DIRECTION('',(0.,-1.,0.));
#11336=DIRECTION('center_axis',(0.,-1.,0.));
#11337=DIRECTION('ref_axis',(0.,0.,-1.));
#11338=DIRECTION('',(0.,-1.,0.));
#11339=DIRECTION('center_axis',(0.,1.,0.));
#11340=DIRECTION('ref_axis',(0.,0.,1.));
#11341=DIRECTION('center_axis',(0.,-1.,0.));
#11342=DIRECTION('ref_axis',(0.,0.,-1.));
#11343=DIRECTION('',(0.,-1.,0.));
#11344=DIRECTION('center_axis',(0.,-1.,0.));
#11345=DIRECTION('ref_axis',(0.,0.,-1.));
#11346=DIRECTION('',(0.,-1.,0.));
#11347=DIRECTION('center_axis',(0.,1.,0.));
#11348=DIRECTION('ref_axis',(0.,0.,1.));
#11349=DIRECTION('center_axis',(0.,-1.,0.));
#11350=DIRECTION('ref_axis',(0.,0.,-1.));
#11351=DIRECTION('',(0.,-1.,0.));
#11352=DIRECTION('center_axis',(0.,-1.,0.));
#11353=DIRECTION('ref_axis',(0.,0.,-1.));
#11354=DIRECTION('',(0.,-1.,0.));
#11355=DIRECTION('center_axis',(0.,1.,0.));
#11356=DIRECTION('ref_axis',(0.,0.,1.));
#11357=DIRECTION('center_axis',(0.,-1.,0.));
#11358=DIRECTION('ref_axis',(0.,0.,-1.));
#11359=DIRECTION('',(0.,-1.,0.));
#11360=DIRECTION('center_axis',(0.,-1.,0.));
#11361=DIRECTION('ref_axis',(0.,0.,-1.));
#11362=DIRECTION('',(0.,-1.,0.));
#11363=DIRECTION('center_axis',(0.,1.,0.));
#11364=DIRECTION('ref_axis',(0.,0.,1.));
#11365=DIRECTION('center_axis',(0.,-1.,0.));
#11366=DIRECTION('ref_axis',(0.,0.,-1.));
#11367=DIRECTION('',(0.,-1.,0.));
#11368=DIRECTION('center_axis',(0.,-1.,0.));
#11369=DIRECTION('ref_axis',(0.,0.,-1.));
#11370=DIRECTION('',(0.,-1.,0.));
#11371=DIRECTION('center_axis',(0.,1.,0.));
#11372=DIRECTION('ref_axis',(0.,0.,1.));
#11373=DIRECTION('center_axis',(0.,-1.,0.));
#11374=DIRECTION('ref_axis',(0.,0.,-1.));
#11375=DIRECTION('',(0.,-1.,0.));
#11376=DIRECTION('center_axis',(0.,-1.,0.));
#11377=DIRECTION('ref_axis',(0.,0.,-1.));
#11378=DIRECTION('',(0.,-1.,0.));
#11379=DIRECTION('center_axis',(0.,1.,0.));
#11380=DIRECTION('ref_axis',(0.,0.,1.));
#11381=DIRECTION('center_axis',(0.,-1.,0.));
#11382=DIRECTION('ref_axis',(0.,0.,-1.));
#11383=DIRECTION('',(0.,-1.,0.));
#11384=DIRECTION('center_axis',(0.,-1.,0.));
#11385=DIRECTION('ref_axis',(0.,0.,-1.));
#11386=DIRECTION('',(0.,-1.,0.));
#11387=DIRECTION('center_axis',(0.,1.,0.));
#11388=DIRECTION('ref_axis',(0.,0.,1.));
#11389=DIRECTION('center_axis',(0.,-1.,0.));
#11390=DIRECTION('ref_axis',(0.,0.,-1.));
#11391=DIRECTION('',(0.,-1.,0.));
#11392=DIRECTION('center_axis',(0.,-1.,0.));
#11393=DIRECTION('ref_axis',(0.,0.,-1.));
#11394=DIRECTION('',(0.,-1.,0.));
#11395=DIRECTION('center_axis',(0.,1.,0.));
#11396=DIRECTION('ref_axis',(0.,0.,1.));
#11397=DIRECTION('center_axis',(0.,-1.,0.));
#11398=DIRECTION('ref_axis',(0.,0.,-1.));
#11399=DIRECTION('',(0.,-1.,0.));
#11400=DIRECTION('center_axis',(0.,-1.,0.));
#11401=DIRECTION('ref_axis',(0.,0.,-1.));
#11402=DIRECTION('',(0.,-1.,0.));
#11403=DIRECTION('center_axis',(0.,1.,0.));
#11404=DIRECTION('ref_axis',(0.,0.,1.));
#11405=DIRECTION('center_axis',(0.,-1.,0.));
#11406=DIRECTION('ref_axis',(0.,0.,-1.));
#11407=DIRECTION('',(0.,-1.,0.));
#11408=DIRECTION('center_axis',(0.,-1.,0.));
#11409=DIRECTION('ref_axis',(0.,0.,-1.));
#11410=DIRECTION('',(0.,-1.,0.));
#11411=DIRECTION('center_axis',(0.,1.,0.));
#11412=DIRECTION('ref_axis',(0.,0.,1.));
#11413=DIRECTION('center_axis',(0.,-1.,0.));
#11414=DIRECTION('ref_axis',(0.,0.,-1.));
#11415=DIRECTION('',(0.,-1.,0.));
#11416=DIRECTION('center_axis',(0.,-1.,0.));
#11417=DIRECTION('ref_axis',(0.,0.,-1.));
#11418=DIRECTION('',(0.,-1.,0.));
#11419=DIRECTION('center_axis',(0.,1.,0.));
#11420=DIRECTION('ref_axis',(0.,0.,1.));
#11421=DIRECTION('center_axis',(0.,-1.,0.));
#11422=DIRECTION('ref_axis',(0.,0.,-1.));
#11423=DIRECTION('',(0.,-1.,0.));
#11424=DIRECTION('center_axis',(0.,-1.,0.));
#11425=DIRECTION('ref_axis',(0.,0.,-1.));
#11426=DIRECTION('',(0.,-1.,0.));
#11427=DIRECTION('center_axis',(0.,1.,0.));
#11428=DIRECTION('ref_axis',(0.,0.,1.));
#11429=DIRECTION('center_axis',(0.,-1.,0.));
#11430=DIRECTION('ref_axis',(0.,0.,-1.));
#11431=DIRECTION('',(0.,-1.,0.));
#11432=DIRECTION('center_axis',(0.,-1.,0.));
#11433=DIRECTION('ref_axis',(0.,0.,-1.));
#11434=DIRECTION('',(0.,-1.,0.));
#11435=DIRECTION('center_axis',(0.,1.,0.));
#11436=DIRECTION('ref_axis',(0.,0.,1.));
#11437=DIRECTION('center_axis',(0.,-1.,0.));
#11438=DIRECTION('ref_axis',(0.,0.,-1.));
#11439=DIRECTION('',(0.,-1.,0.));
#11440=DIRECTION('center_axis',(0.,-1.,0.));
#11441=DIRECTION('ref_axis',(0.,0.,-1.));
#11442=DIRECTION('',(0.,-1.,0.));
#11443=DIRECTION('center_axis',(0.,1.,0.));
#11444=DIRECTION('ref_axis',(0.,0.,1.));
#11445=DIRECTION('center_axis',(0.,-1.,0.));
#11446=DIRECTION('ref_axis',(0.,0.,-1.));
#11447=DIRECTION('',(0.,-1.,0.));
#11448=DIRECTION('center_axis',(0.,-1.,0.));
#11449=DIRECTION('ref_axis',(0.,0.,-1.));
#11450=DIRECTION('',(0.,-1.,0.));
#11451=DIRECTION('center_axis',(0.,1.,0.));
#11452=DIRECTION('ref_axis',(0.,0.,1.));
#11453=DIRECTION('center_axis',(0.,-1.,0.));
#11454=DIRECTION('ref_axis',(0.,0.,-1.));
#11455=DIRECTION('',(0.,-1.,0.));
#11456=DIRECTION('center_axis',(0.,-1.,0.));
#11457=DIRECTION('ref_axis',(0.,0.,-1.));
#11458=DIRECTION('',(0.,-1.,0.));
#11459=DIRECTION('center_axis',(0.,1.,0.));
#11460=DIRECTION('ref_axis',(0.,0.,1.));
#11461=DIRECTION('center_axis',(0.,-1.,0.));
#11462=DIRECTION('ref_axis',(0.,0.,-1.));
#11463=DIRECTION('',(0.,-1.,0.));
#11464=DIRECTION('center_axis',(0.,-1.,0.));
#11465=DIRECTION('ref_axis',(0.,0.,-1.));
#11466=DIRECTION('',(0.,-1.,0.));
#11467=DIRECTION('center_axis',(0.,1.,0.));
#11468=DIRECTION('ref_axis',(0.,0.,1.));
#11469=DIRECTION('center_axis',(0.,-1.,0.));
#11470=DIRECTION('ref_axis',(0.,0.,-1.));
#11471=DIRECTION('',(0.,-1.,0.));
#11472=DIRECTION('center_axis',(0.,-1.,0.));
#11473=DIRECTION('ref_axis',(0.,0.,-1.));
#11474=DIRECTION('',(0.,-1.,0.));
#11475=DIRECTION('center_axis',(0.,1.,0.));
#11476=DIRECTION('ref_axis',(0.,0.,1.));
#11477=DIRECTION('center_axis',(0.,-1.,0.));
#11478=DIRECTION('ref_axis',(0.,0.,-1.));
#11479=DIRECTION('',(0.,-1.,0.));
#11480=DIRECTION('center_axis',(0.,-1.,0.));
#11481=DIRECTION('ref_axis',(0.,0.,-1.));
#11482=DIRECTION('',(0.,-1.,0.));
#11483=DIRECTION('center_axis',(0.,1.,0.));
#11484=DIRECTION('ref_axis',(0.,0.,1.));
#11485=DIRECTION('center_axis',(0.,-1.,0.));
#11486=DIRECTION('ref_axis',(0.,0.,-1.));
#11487=DIRECTION('',(0.,-1.,0.));
#11488=DIRECTION('center_axis',(0.,-1.,0.));
#11489=DIRECTION('ref_axis',(0.,0.,-1.));
#11490=DIRECTION('',(0.,-1.,0.));
#11491=DIRECTION('center_axis',(0.,1.,0.));
#11492=DIRECTION('ref_axis',(0.,0.,1.));
#11493=DIRECTION('center_axis',(0.,-1.,0.));
#11494=DIRECTION('ref_axis',(0.,0.,-1.));
#11495=DIRECTION('',(0.,-1.,0.));
#11496=DIRECTION('center_axis',(0.,-1.,0.));
#11497=DIRECTION('ref_axis',(0.,0.,-1.));
#11498=DIRECTION('',(0.,-1.,0.));
#11499=DIRECTION('center_axis',(0.,1.,0.));
#11500=DIRECTION('ref_axis',(0.,0.,1.));
#11501=DIRECTION('center_axis',(0.,-1.,0.));
#11502=DIRECTION('ref_axis',(0.,0.,-1.));
#11503=DIRECTION('',(0.,-1.,0.));
#11504=DIRECTION('center_axis',(0.,-1.,0.));
#11505=DIRECTION('ref_axis',(0.,0.,-1.));
#11506=DIRECTION('',(0.,-1.,0.));
#11507=DIRECTION('center_axis',(0.,1.,0.));
#11508=DIRECTION('ref_axis',(0.,0.,1.));
#11509=DIRECTION('center_axis',(0.,-1.,0.));
#11510=DIRECTION('ref_axis',(0.,0.,-1.));
#11511=DIRECTION('',(0.,-1.,0.));
#11512=DIRECTION('center_axis',(0.,-1.,0.));
#11513=DIRECTION('ref_axis',(0.,0.,-1.));
#11514=DIRECTION('',(0.,-1.,0.));
#11515=DIRECTION('center_axis',(0.,1.,0.));
#11516=DIRECTION('ref_axis',(0.,0.,1.));
#11517=DIRECTION('center_axis',(0.,-1.,0.));
#11518=DIRECTION('ref_axis',(0.,0.,-1.));
#11519=DIRECTION('',(0.,-1.,0.));
#11520=DIRECTION('center_axis',(0.,-1.,0.));
#11521=DIRECTION('ref_axis',(0.,0.,-1.));
#11522=DIRECTION('',(0.,-1.,0.));
#11523=DIRECTION('center_axis',(0.,1.,0.));
#11524=DIRECTION('ref_axis',(0.,0.,1.));
#11525=DIRECTION('center_axis',(0.,-1.,0.));
#11526=DIRECTION('ref_axis',(0.,0.,-1.));
#11527=DIRECTION('',(0.,-1.,0.));
#11528=DIRECTION('center_axis',(0.,-1.,0.));
#11529=DIRECTION('ref_axis',(0.,0.,-1.));
#11530=DIRECTION('',(0.,-1.,0.));
#11531=DIRECTION('center_axis',(0.,1.,0.));
#11532=DIRECTION('ref_axis',(0.,0.,1.));
#11533=DIRECTION('center_axis',(0.,-1.,0.));
#11534=DIRECTION('ref_axis',(0.,0.,-1.));
#11535=DIRECTION('',(0.,-1.,0.));
#11536=DIRECTION('center_axis',(0.,-1.,0.));
#11537=DIRECTION('ref_axis',(0.,0.,-1.));
#11538=DIRECTION('',(0.,-1.,0.));
#11539=DIRECTION('center_axis',(0.,1.,0.));
#11540=DIRECTION('ref_axis',(0.,0.,1.));
#11541=DIRECTION('center_axis',(0.,-1.,0.));
#11542=DIRECTION('ref_axis',(0.,0.,-1.));
#11543=DIRECTION('',(0.,-1.,0.));
#11544=DIRECTION('center_axis',(0.,-1.,0.));
#11545=DIRECTION('ref_axis',(0.,0.,-1.));
#11546=DIRECTION('',(0.,-1.,0.));
#11547=DIRECTION('center_axis',(0.,1.,0.));
#11548=DIRECTION('ref_axis',(0.,0.,1.));
#11549=DIRECTION('center_axis',(0.,-1.,0.));
#11550=DIRECTION('ref_axis',(0.,0.,-1.));
#11551=DIRECTION('',(0.,-1.,0.));
#11552=DIRECTION('center_axis',(0.,-1.,0.));
#11553=DIRECTION('ref_axis',(0.,0.,-1.));
#11554=DIRECTION('',(0.,-1.,0.));
#11555=DIRECTION('center_axis',(0.,1.,0.));
#11556=DIRECTION('ref_axis',(0.,0.,1.));
#11557=DIRECTION('center_axis',(0.598674156532674,0.,0.800992668068748));
#11558=DIRECTION('ref_axis',(0.800992668068748,0.,-0.598674156532674));
#11559=DIRECTION('',(0.800992668068748,0.,-0.598674156532674));
#11560=DIRECTION('',(0.,-1.,0.));
#11561=DIRECTION('',(0.800992668068748,0.,-0.598674156532674));
#11562=DIRECTION('center_axis',(-0.598674156532673,0.,0.800992668068749));
#11563=DIRECTION('ref_axis',(0.800992668068749,0.,0.598674156532673));
#11564=DIRECTION('',(0.800992668068749,0.,0.598674156532673));
#11565=DIRECTION('',(0.800992668068749,0.,0.598674156532673));
#11566=DIRECTION('center_axis',(0.716606343753432,0.,0.697477847743093));
#11567=DIRECTION('ref_axis',(0.697477847743093,0.,-0.716606343753432));
#11568=DIRECTION('',(0.697477847743093,0.,-0.716606343753432));
#11569=DIRECTION('',(0.,-1.,0.));
#11570=DIRECTION('',(0.697477847743093,0.,-0.716606343753432));
#11571=DIRECTION('center_axis',(-0.466000624692467,0.,0.884784390564295));
#11572=DIRECTION('ref_axis',(0.884784390564295,0.,0.466000624692467));
#11573=DIRECTION('',(0.884784390564295,0.,0.466000624692467));
#11574=DIRECTION('',(0.884784390564295,0.,0.466000624692467));
#11575=DIRECTION('center_axis',(0.816893304510879,0.,0.57678880800974));
#11576=DIRECTION('ref_axis',(0.57678880800974,0.,-0.816893304510879));
#11577=DIRECTION('',(0.57678880800974,0.,-0.816893304510879));
#11578=DIRECTION('',(0.,-1.,0.));
#11579=DIRECTION('',(0.57678880800974,0.,-0.816893304510879));
#11580=DIRECTION('center_axis',(-0.321852610904928,0.,0.946789784933108));
#11581=DIRECTION('ref_axis',(0.946789784933108,0.,0.321852610904928));
#11582=DIRECTION('',(0.946789784933108,0.,0.321852610904928));
#11583=DIRECTION('',(0.946789784933108,0.,0.321852610904928));
#11584=DIRECTION('center_axis',(0.897065640997825,0.,0.441897313570881));
#11585=DIRECTION('ref_axis',(0.441897313570881,0.,-0.897065640997825));
#11586=DIRECTION('',(0.441897313570881,0.,-0.897065640997825));
#11587=DIRECTION('',(0.,-1.,0.));
#11588=DIRECTION('',(0.441897313570881,0.,-0.897065640997825));
#11589=DIRECTION('center_axis',(-0.169779517669335,0.,0.985482072581723));
#11590=DIRECTION('ref_axis',(0.985482072581723,0.,0.169779517669335));
#11591=DIRECTION('',(0.985482072581723,0.,0.169779517669335));
#11592=DIRECTION('',(0.985482072581723,0.,0.169779517669335));
#11593=DIRECTION('center_axis',(0.955149244213231,0.,0.296124840698806));
#11594=DIRECTION('ref_axis',(0.296124840698806,0.,-0.955149244213231));
#11595=DIRECTION('',(0.296124840698806,0.,-0.955149244213231));
#11596=DIRECTION('',(0.,-1.,0.));
#11597=DIRECTION('',(0.296124840698806,0.,-0.955149244213231));
#11598=DIRECTION('center_axis',(-0.013525889242808,0.,0.99990852097589));
#11599=DIRECTION('ref_axis',(0.99990852097589,0.,0.013525889242808));
#11600=DIRECTION('',(0.99990852097589,0.,0.013525889242808));
#11601=DIRECTION('',(0.99990852097589,0.,0.013525889242808));
#11602=DIRECTION('center_axis',(0.989713903077508,0.,0.143060791466725));
#11603=DIRECTION('ref_axis',(0.143060791466725,0.,-0.989713903077508));
#11604=DIRECTION('',(0.143060791466725,0.,-0.989713903077508));
#11605=DIRECTION('',(0.,-1.,0.));
#11606=DIRECTION('',(0.143060791466725,0.,-0.989713903077508));
#11607=DIRECTION('center_axis',(0.143060791466729,0.,0.989713903077507));
#11608=DIRECTION('ref_axis',(0.989713903077507,0.,-0.143060791466729));
#11609=DIRECTION('',(0.989713903077507,0.,-0.143060791466729));
#11610=DIRECTION('',(0.989713903077507,0.,-0.143060791466729));
#11611=DIRECTION('center_axis',(0.99990852097589,0.,-0.0135258892428123));
#11612=DIRECTION('ref_axis',(-0.0135258892428123,0.,-0.99990852097589));
#11613=DIRECTION('',(-0.0135258892428123,0.,-0.99990852097589));
#11614=DIRECTION('',(0.,-1.,0.));
#11615=DIRECTION('',(-0.0135258892428123,0.,-0.99990852097589));
#11616=DIRECTION('center_axis',(0.29612484069881,0.,0.95514924421323));
#11617=DIRECTION('ref_axis',(0.95514924421323,0.,-0.29612484069881));
#11618=DIRECTION('',(0.95514924421323,0.,-0.29612484069881));
#11619=DIRECTION('',(0.95514924421323,0.,-0.29612484069881));
#11620=DIRECTION('center_axis',(0.985482072581722,0.,-0.169779517669339));
#11621=DIRECTION('ref_axis',(-0.169779517669339,0.,-0.985482072581722));
#11622=DIRECTION('',(-0.169779517669339,0.,-0.985482072581722));
#11623=DIRECTION('',(0.,-1.,0.));
#11624=DIRECTION('',(-0.169779517669339,0.,-0.985482072581722));
#11625=DIRECTION('center_axis',(0.441897313570885,0.,0.897065640997823));
#11626=DIRECTION('ref_axis',(0.897065640997823,0.,-0.441897313570885));
#11627=DIRECTION('',(0.897065640997823,0.,-0.441897313570885));
#11628=DIRECTION('',(0.897065640997823,0.,-0.441897313570885));
#11629=DIRECTION('center_axis',(0.946789784933107,0.,-0.321852610904932));
#11630=DIRECTION('ref_axis',(-0.321852610904932,0.,-0.946789784933107));
#11631=DIRECTION('',(-0.321852610904932,0.,-0.946789784933107));
#11632=DIRECTION('',(0.,-1.,0.));
#11633=DIRECTION('',(-0.321852610904932,0.,-0.946789784933107));
#11634=DIRECTION('center_axis',(0.576788808009743,0.,0.816893304510877));
#11635=DIRECTION('ref_axis',(0.816893304510876,0.,-0.576788808009743));
#11636=DIRECTION('',(0.816893304510877,0.,-0.576788808009743));
#11637=DIRECTION('',(0.816893304510877,0.,-0.576788808009743));
#11638=DIRECTION('center_axis',(0.884784390564293,0.,-0.466000624692471));
#11639=DIRECTION('ref_axis',(-0.466000624692471,0.,-0.884784390564292));
#11640=DIRECTION('',(-0.466000624692471,0.,-0.884784390564293));
#11641=DIRECTION('',(0.,-1.,0.));
#11642=DIRECTION('',(-0.466000624692471,0.,-0.884784390564293));
#11643=DIRECTION('center_axis',(0.697477847743097,0.,0.716606343753429));
#11644=DIRECTION('ref_axis',(0.716606343753429,0.,-0.697477847743097));
#11645=DIRECTION('',(0.716606343753429,0.,-0.697477847743097));
#11646=DIRECTION('',(0.716606343753429,0.,-0.697477847743097));
#11647=DIRECTION('center_axis',(0.800992668068746,0.,-0.598674156532677));
#11648=DIRECTION('ref_axis',(-0.598674156532677,0.,-0.800992668068746));
#11649=DIRECTION('',(-0.598674156532677,0.,-0.800992668068746));
#11650=DIRECTION('',(0.,-1.,0.));
#11651=DIRECTION('',(-0.598674156532677,0.,-0.800992668068746));
#11652=DIRECTION('center_axis',(0.800992668068751,0.,0.59867415653267));
#11653=DIRECTION('ref_axis',(0.59867415653267,0.,-0.800992668068751));
#11654=DIRECTION('',(0.59867415653267,0.,-0.800992668068751));
#11655=DIRECTION('',(0.59867415653267,0.,-0.800992668068751));
#11656=DIRECTION('center_axis',(0.697477847743091,0.,-0.716606343753435));
#11657=DIRECTION('ref_axis',(-0.716606343753435,0.,-0.697477847743091));
#11658=DIRECTION('',(-0.716606343753435,0.,-0.697477847743091));
#11659=DIRECTION('',(0.,-1.,0.));
#11660=DIRECTION('',(-0.716606343753435,0.,-0.697477847743091));
#11661=DIRECTION('center_axis',(0.884784390564296,0.,0.466000624692464));
#11662=DIRECTION('ref_axis',(0.466000624692464,0.,-0.884784390564296));
#11663=DIRECTION('',(0.466000624692464,0.,-0.884784390564296));
#11664=DIRECTION('',(0.466000624692464,0.,-0.884784390564296));
#11665=DIRECTION('center_axis',(0.576788808009737,0.,-0.816893304510881));
#11666=DIRECTION('ref_axis',(-0.816893304510881,0.,-0.576788808009737));
#11667=DIRECTION('',(-0.816893304510881,0.,-0.576788808009737));
#11668=DIRECTION('',(0.,-1.,0.));
#11669=DIRECTION('',(-0.816893304510881,0.,-0.576788808009737));
#11670=DIRECTION('center_axis',(0.946789784933109,0.,0.321852610904925));
#11671=DIRECTION('ref_axis',(0.321852610904925,0.,-0.946789784933109));
#11672=DIRECTION('',(0.321852610904925,0.,-0.946789784933109));
#11673=DIRECTION('',(0.321852610904925,0.,-0.946789784933109));
#11674=DIRECTION('center_axis',(0.441897313570878,0.,-0.897065640997826));
#11675=DIRECTION('ref_axis',(-0.897065640997827,0.,-0.441897313570878));
#11676=DIRECTION('',(-0.897065640997826,0.,-0.441897313570878));
#11677=DIRECTION('',(0.,-1.,0.));
#11678=DIRECTION('',(-0.897065640997826,0.,-0.441897313570878));
#11679=DIRECTION('center_axis',(0.985482072581723,0.,0.169779517669331));
#11680=DIRECTION('ref_axis',(0.169779517669331,0.,-0.985482072581724));
#11681=DIRECTION('',(0.169779517669331,0.,-0.985482072581723));
#11682=DIRECTION('',(0.169779517669331,0.,-0.985482072581723));
#11683=DIRECTION('center_axis',(0.296124840698803,0.,-0.955149244213232));
#11684=DIRECTION('ref_axis',(-0.955149244213232,0.,-0.296124840698803));
#11685=DIRECTION('',(-0.955149244213232,0.,-0.296124840698803));
#11686=DIRECTION('',(0.,-1.,0.));
#11687=DIRECTION('',(-0.955149244213232,0.,-0.296124840698803));
#11688=DIRECTION('center_axis',(0.99990852097589,0.,0.0135258892428046));
#11689=DIRECTION('ref_axis',(0.0135258892428046,0.,-0.99990852097589));
#11690=DIRECTION('',(0.0135258892428046,0.,-0.99990852097589));
#11691=DIRECTION('',(0.0135258892428046,0.,-0.99990852097589));
#11692=DIRECTION('center_axis',(0.143060791466722,0.,-0.989713903077508));
#11693=DIRECTION('ref_axis',(-0.989713903077508,0.,-0.143060791466722));
#11694=DIRECTION('',(-0.989713903077508,0.,-0.143060791466722));
#11695=DIRECTION('',(0.,-1.,0.));
#11696=DIRECTION('',(-0.989713903077508,0.,-0.143060791466722));
#11697=DIRECTION('center_axis',(0.989713903077507,0.,-0.143060791466733));
#11698=DIRECTION('ref_axis',(-0.143060791466733,0.,-0.989713903077507));
#11699=DIRECTION('',(-0.143060791466733,0.,-0.989713903077507));
#11700=DIRECTION('',(-0.143060791466733,0.,-0.989713903077507));
#11701=DIRECTION('center_axis',(-0.0135258892428158,0.,-0.99990852097589));
#11702=DIRECTION('ref_axis',(-0.99990852097589,0.,0.0135258892428158));
#11703=DIRECTION('',(-0.99990852097589,0.,0.0135258892428158));
#11704=DIRECTION('',(0.,-1.,0.));
#11705=DIRECTION('',(-0.99990852097589,0.,0.0135258892428158));
#11706=DIRECTION('center_axis',(0.955149244213229,0.,-0.296124840698814));
#11707=DIRECTION('ref_axis',(-0.296124840698814,0.,-0.955149244213229));
#11708=DIRECTION('',(-0.296124840698814,0.,-0.955149244213229));
#11709=DIRECTION('',(-0.296124840698814,0.,-0.955149244213229));
#11710=DIRECTION('center_axis',(-0.169779517669343,0.,-0.985482072581721));
#11711=DIRECTION('ref_axis',(-0.985482072581721,0.,0.169779517669343));
#11712=DIRECTION('',(-0.985482072581721,0.,0.169779517669343));
#11713=DIRECTION('',(0.,-1.,0.));
#11714=DIRECTION('',(-0.985482072581721,0.,0.169779517669343));
#11715=DIRECTION('center_axis',(0.897065640997821,0.,-0.441897313570888));
#11716=DIRECTION('ref_axis',(-0.441897313570888,0.,-0.897065640997821));
#11717=DIRECTION('',(-0.441897313570888,0.,-0.897065640997821));
#11718=DIRECTION('',(-0.441897313570888,0.,-0.897065640997821));
#11719=DIRECTION('center_axis',(-0.321852610904936,0.,-0.946789784933105));
#11720=DIRECTION('ref_axis',(-0.946789784933106,0.,0.321852610904936));
#11721=DIRECTION('',(-0.946789784933105,0.,0.321852610904936));
#11722=DIRECTION('',(0.,-1.,0.));
#11723=DIRECTION('',(-0.946789784933105,0.,0.321852610904936));
#11724=DIRECTION('center_axis',(0.816893304510874,0.,-0.576788808009746));
#11725=DIRECTION('ref_axis',(-0.576788808009746,0.,-0.816893304510874));
#11726=DIRECTION('',(-0.576788808009746,0.,-0.816893304510874));
#11727=DIRECTION('',(-0.576788808009746,0.,-0.816893304510874));
#11728=DIRECTION('center_axis',(-0.466000624692474,0.,-0.884784390564291));
#11729=DIRECTION('ref_axis',(-0.884784390564291,0.,0.466000624692474));
#11730=DIRECTION('',(-0.884784390564291,0.,0.466000624692474));
#11731=DIRECTION('',(0.,-1.,0.));
#11732=DIRECTION('',(-0.884784390564291,0.,0.466000624692474));
#11733=DIRECTION('center_axis',(0.716606343753427,0.,-0.697477847743099));
#11734=DIRECTION('ref_axis',(-0.697477847743099,0.,-0.716606343753427));
#11735=DIRECTION('',(-0.697477847743099,0.,-0.716606343753427));
#11736=DIRECTION('',(-0.697477847743099,0.,-0.716606343753427));
#11737=DIRECTION('center_axis',(-0.598674156532674,0.,-0.800992668068748));
#11738=DIRECTION('ref_axis',(-0.800992668068748,0.,0.598674156532674));
#11739=DIRECTION('',(-0.800992668068748,0.,0.598674156532674));
#11740=DIRECTION('',(0.,-1.,0.));
#11741=DIRECTION('',(-0.800992668068748,0.,0.598674156532674));
#11742=DIRECTION('center_axis',(0.598674156532673,0.,-0.800992668068749));
#11743=DIRECTION('ref_axis',(-0.800992668068749,0.,-0.598674156532673));
#11744=DIRECTION('',(-0.800992668068749,0.,-0.598674156532673));
#11745=DIRECTION('',(-0.800992668068749,0.,-0.598674156532673));
#11746=DIRECTION('center_axis',(-0.716606343753437,0.,-0.697477847743088));
#11747=DIRECTION('ref_axis',(-0.697477847743088,0.,0.716606343753437));
#11748=DIRECTION('',(-0.697477847743088,0.,0.716606343753437));
#11749=DIRECTION('',(0.,-1.,0.));
#11750=DIRECTION('',(-0.697477847743088,0.,0.716606343753437));
#11751=DIRECTION('center_axis',(0.466000624692461,0.,-0.884784390564298));
#11752=DIRECTION('ref_axis',(-0.884784390564298,0.,-0.466000624692461));
#11753=DIRECTION('',(-0.884784390564298,0.,-0.466000624692461));
#11754=DIRECTION('',(-0.884784390564298,0.,-0.466000624692461));
#11755=DIRECTION('center_axis',(-0.816893304510883,0.,-0.576788808009734));
#11756=DIRECTION('ref_axis',(-0.576788808009734,0.,0.816893304510883));
#11757=DIRECTION('',(-0.576788808009734,0.,0.816893304510883));
#11758=DIRECTION('',(0.,-1.,0.));
#11759=DIRECTION('',(-0.576788808009734,0.,0.816893304510883));
#11760=DIRECTION('center_axis',(0.321852610904921,0.,-0.94678978493311));
#11761=DIRECTION('ref_axis',(-0.94678978493311,0.,-0.321852610904921));
#11762=DIRECTION('',(-0.94678978493311,0.,-0.321852610904921));
#11763=DIRECTION('',(-0.94678978493311,0.,-0.321852610904921));
#11764=DIRECTION('center_axis',(-0.897065640997828,0.,-0.441897313570875));
#11765=DIRECTION('ref_axis',(-0.441897313570875,0.,0.897065640997828));
#11766=DIRECTION('',(-0.441897313570875,0.,0.897065640997828));
#11767=DIRECTION('',(0.,-1.,0.));
#11768=DIRECTION('',(-0.441897313570875,0.,0.897065640997828));
#11769=DIRECTION('center_axis',(0.169779517669328,0.,-0.985482072581724));
#11770=DIRECTION('ref_axis',(-0.985482072581724,0.,-0.169779517669328));
#11771=DIRECTION('',(-0.985482072581724,0.,-0.169779517669328));
#11772=DIRECTION('',(-0.985482072581724,0.,-0.169779517669328));
#11773=DIRECTION('center_axis',(-0.955149244213233,0.,-0.296124840698799));
#11774=DIRECTION('ref_axis',(-0.296124840698799,0.,0.955149244213233));
#11775=DIRECTION('',(-0.296124840698799,0.,0.955149244213233));
#11776=DIRECTION('',(0.,-1.,0.));
#11777=DIRECTION('',(-0.296124840698799,0.,0.955149244213233));
#11778=DIRECTION('center_axis',(0.0135258892428006,0.,-0.99990852097589));
#11779=DIRECTION('ref_axis',(-0.99990852097589,0.,-0.0135258892428006));
#11780=DIRECTION('',(-0.99990852097589,0.,-0.0135258892428006));
#11781=DIRECTION('',(-0.99990852097589,0.,-0.0135258892428006));
#11782=DIRECTION('center_axis',(-0.989713903077509,0.,-0.143060791466718));
#11783=DIRECTION('ref_axis',(-0.143060791466718,0.,0.989713903077509));
#11784=DIRECTION('',(-0.143060791466718,0.,0.989713903077509));
#11785=DIRECTION('',(0.,-1.,0.));
#11786=DIRECTION('',(-0.143060791466718,0.,0.989713903077509));
#11787=DIRECTION('center_axis',(-0.143060791466736,0.,-0.989713903077506));
#11788=DIRECTION('ref_axis',(-0.989713903077506,0.,0.143060791466736));
#11789=DIRECTION('',(-0.989713903077506,0.,0.143060791466736));
#11790=DIRECTION('',(-0.989713903077506,0.,0.143060791466736));
#11791=DIRECTION('center_axis',(-0.99990852097589,0.,0.0135258892428198));
#11792=DIRECTION('ref_axis',(0.0135258892428198,0.,0.99990852097589));
#11793=DIRECTION('',(0.0135258892428198,0.,0.99990852097589));
#11794=DIRECTION('',(0.,-1.,0.));
#11795=DIRECTION('',(0.0135258892428198,0.,0.99990852097589));
#11796=DIRECTION('center_axis',(-0.296124840698817,0.,-0.955149244213228));
#11797=DIRECTION('ref_axis',(-0.955149244213228,0.,0.296124840698817));
#11798=DIRECTION('',(-0.955149244213228,0.,0.296124840698817));
#11799=DIRECTION('',(-0.955149244213228,0.,0.296124840698817));
#11800=DIRECTION('center_axis',(-0.985482072581721,0.,0.169779517669346));
#11801=DIRECTION('ref_axis',(0.169779517669346,0.,0.985482072581721));
#11802=DIRECTION('',(0.169779517669346,0.,0.985482072581721));
#11803=DIRECTION('',(0.,-1.,0.));
#11804=DIRECTION('',(0.169779517669346,0.,0.985482072581721));
#11805=DIRECTION('center_axis',(-0.441897313570892,0.,-0.89706564099782));
#11806=DIRECTION('ref_axis',(-0.89706564099782,0.,0.441897313570891));
#11807=DIRECTION('',(-0.89706564099782,0.,0.441897313570891));
#11808=DIRECTION('',(-0.89706564099782,0.,0.441897313570891));
#11809=DIRECTION('center_axis',(-0.946789784933104,0.,0.321852610904939));
#11810=DIRECTION('ref_axis',(0.321852610904939,0.,0.946789784933104));
#11811=DIRECTION('',(0.321852610904939,0.,0.946789784933104));
#11812=DIRECTION('',(0.,-1.,0.));
#11813=DIRECTION('',(0.321852610904939,0.,0.946789784933104));
#11814=DIRECTION('center_axis',(-0.576788808009749,0.,-0.816893304510873));
#11815=DIRECTION('ref_axis',(-0.816893304510873,0.,0.576788808009749));
#11816=DIRECTION('',(-0.816893304510873,0.,0.576788808009749));
#11817=DIRECTION('',(-0.816893304510873,0.,0.576788808009749));
#11818=DIRECTION('center_axis',(-0.884784390564289,0.,0.466000624692478));
#11819=DIRECTION('ref_axis',(0.466000624692478,0.,0.884784390564289));
#11820=DIRECTION('',(0.466000624692478,0.,0.884784390564289));
#11821=DIRECTION('',(0.,-1.,0.));
#11822=DIRECTION('',(0.466000624692478,0.,0.884784390564289));
#11823=DIRECTION('center_axis',(-0.697477847743102,0.,-0.716606343753424));
#11824=DIRECTION('ref_axis',(-0.716606343753424,0.,0.697477847743102));
#11825=DIRECTION('',(-0.716606343753424,0.,0.697477847743102));
#11826=DIRECTION('',(-0.716606343753424,0.,0.697477847743102));
#11827=DIRECTION('center_axis',(-0.800992668068742,0.,0.598674156532682));
#11828=DIRECTION('ref_axis',(0.598674156532682,0.,0.800992668068742));
#11829=DIRECTION('',(0.598674156532682,0.,0.800992668068742));
#11830=DIRECTION('',(0.,-1.,0.));
#11831=DIRECTION('',(0.598674156532682,0.,0.800992668068742));
#11832=DIRECTION('center_axis',(-0.800992668068755,0.,-0.598674156532665));
#11833=DIRECTION('ref_axis',(-0.598674156532665,0.,0.800992668068755));
#11834=DIRECTION('',(-0.598674156532665,0.,0.800992668068755));
#11835=DIRECTION('',(-0.598674156532665,0.,0.800992668068755));
#11836=DIRECTION('center_axis',(-0.697477847743086,0.,0.71660634375344));
#11837=DIRECTION('ref_axis',(0.71660634375344,0.,0.697477847743086));
#11838=DIRECTION('',(0.71660634375344,0.,0.697477847743086));
#11839=DIRECTION('',(0.,-1.,0.));
#11840=DIRECTION('',(0.71660634375344,0.,0.697477847743086));
#11841=DIRECTION('center_axis',(-0.8847843905643,0.,-0.466000624692458));
#11842=DIRECTION('ref_axis',(-0.466000624692458,0.,0.8847843905643));
#11843=DIRECTION('',(-0.466000624692458,0.,0.8847843905643));
#11844=DIRECTION('',(-0.466000624692458,0.,0.8847843905643));
#11845=DIRECTION('center_axis',(-0.576788808009731,0.,0.816893304510885));
#11846=DIRECTION('ref_axis',(0.816893304510885,0.,0.576788808009731));
#11847=DIRECTION('',(0.816893304510885,0.,0.576788808009731));
#11848=DIRECTION('',(0.,-1.,0.));
#11849=DIRECTION('',(0.816893304510885,0.,0.576788808009731));
#11850=DIRECTION('center_axis',(-0.946789784933112,0.,-0.321852610904918));
#11851=DIRECTION('ref_axis',(-0.321852610904918,0.,0.946789784933112));
#11852=DIRECTION('',(-0.321852610904918,0.,0.946789784933111));
#11853=DIRECTION('',(-0.321852610904918,0.,0.946789784933111));
#11854=DIRECTION('center_axis',(-0.441897313570872,0.,0.897065640997829));
#11855=DIRECTION('ref_axis',(0.897065640997829,0.,0.441897313570872));
#11856=DIRECTION('',(0.897065640997829,0.,0.441897313570872));
#11857=DIRECTION('',(0.,-1.,0.));
#11858=DIRECTION('',(0.897065640997829,0.,0.441897313570872));
#11859=DIRECTION('center_axis',(-0.985482072581725,0.,-0.169779517669325));
#11860=DIRECTION('ref_axis',(-0.169779517669325,0.,0.985482072581725));
#11861=DIRECTION('',(-0.169779517669325,0.,0.985482072581724));
#11862=DIRECTION('',(-0.169779517669325,0.,0.985482072581724));
#11863=DIRECTION('center_axis',(-0.296124840698796,0.,0.955149244213234));
#11864=DIRECTION('ref_axis',(0.955149244213235,0.,0.296124840698796));
#11865=DIRECTION('',(0.955149244213234,0.,0.296124840698796));
#11866=DIRECTION('',(0.,-1.,0.));
#11867=DIRECTION('',(0.955149244213234,0.,0.296124840698796));
#11868=DIRECTION('center_axis',(-0.99990852097589,0.,-0.0135258892427971));
#11869=DIRECTION('ref_axis',(-0.0135258892427971,0.,0.99990852097589));
#11870=DIRECTION('',(-0.0135258892427971,0.,0.99990852097589));
#11871=DIRECTION('',(-0.0135258892427971,0.,0.99990852097589));
#11872=DIRECTION('center_axis',(-0.143060791466715,0.,0.989713903077509));
#11873=DIRECTION('ref_axis',(0.989713903077509,0.,0.143060791466715));
#11874=DIRECTION('',(0.989713903077509,0.,0.143060791466715));
#11875=DIRECTION('',(0.,-1.,0.));
#11876=DIRECTION('',(0.989713903077509,0.,0.143060791466715));
#11877=DIRECTION('center_axis',(-0.989713903077506,0.,0.14306079146674));
#11878=DIRECTION('ref_axis',(0.14306079146674,0.,0.989713903077506));
#11879=DIRECTION('',(0.14306079146674,0.,0.989713903077506));
#11880=DIRECTION('',(0.14306079146674,0.,0.989713903077506));
#11881=DIRECTION('center_axis',(0.0135258892428234,0.,0.99990852097589));
#11882=DIRECTION('ref_axis',(0.99990852097589,0.,-0.0135258892428234));
#11883=DIRECTION('',(0.999908520975889,0.,-0.0135258892428234));
#11884=DIRECTION('',(0.,-1.,0.));
#11885=DIRECTION('',(0.999908520975889,0.,-0.0135258892428234));
#11886=DIRECTION('center_axis',(-0.955149244213227,0.,0.296124840698821));
#11887=DIRECTION('ref_axis',(0.296124840698821,0.,0.955149244213227));
#11888=DIRECTION('',(0.296124840698821,0.,0.955149244213227));
#11889=DIRECTION('',(0.296124840698821,0.,0.955149244213227));
#11890=DIRECTION('center_axis',(0.169779517669349,0.,0.98548207258172));
#11891=DIRECTION('ref_axis',(0.98548207258172,0.,-0.169779517669349));
#11892=DIRECTION('',(0.98548207258172,0.,-0.169779517669349));
#11893=DIRECTION('',(0.,-1.,0.));
#11894=DIRECTION('',(0.98548207258172,0.,-0.169779517669349));
#11895=DIRECTION('center_axis',(-0.897065640997818,0.,0.441897313570894));
#11896=DIRECTION('ref_axis',(0.441897313570895,0.,0.897065640997818));
#11897=DIRECTION('',(0.441897313570894,0.,0.897065640997818));
#11898=DIRECTION('',(0.441897313570894,0.,0.897065640997818));
#11899=DIRECTION('center_axis',(0.321852610904942,0.,0.946789784933103));
#11900=DIRECTION('ref_axis',(0.946789784933103,0.,-0.321852610904942));
#11901=DIRECTION('',(0.946789784933103,0.,-0.321852610904942));
#11902=DIRECTION('',(0.,-1.,0.));
#11903=DIRECTION('',(0.946789784933103,0.,-0.321852610904942));
#11904=DIRECTION('center_axis',(-0.816893304510871,0.,0.576788808009752));
#11905=DIRECTION('ref_axis',(0.576788808009752,0.,0.816893304510871));
#11906=DIRECTION('',(0.576788808009752,0.,0.81689330451087));
#11907=DIRECTION('',(0.576788808009752,0.,0.81689330451087));
#11908=DIRECTION('center_axis',(0.466000624692481,0.,0.884784390564288));
#11909=DIRECTION('ref_axis',(0.884784390564287,0.,-0.466000624692481));
#11910=DIRECTION('',(0.884784390564287,0.,-0.466000624692481));
#11911=DIRECTION('',(0.,-1.,0.));
#11912=DIRECTION('',(0.884784390564287,0.,-0.466000624692481));
#11913=DIRECTION('center_axis',(-0.716606343753422,0.,0.697477847743104));
#11914=DIRECTION('ref_axis',(0.697477847743104,0.,0.716606343753422));
#11915=DIRECTION('',(0.697477847743104,0.,0.716606343753422));
#11916=DIRECTION('',(0.697477847743104,0.,0.716606343753422));
#11917=DIRECTION('center_axis',(0.,-1.,0.));
#11918=DIRECTION('ref_axis',(-1.07806057163162E-14,0.,1.));
#11919=DIRECTION('center_axis',(0.,1.,0.));
#11920=DIRECTION('ref_axis',(0.,0.,1.));
#11921=DIRECTION('center_axis',(0.,-1.,0.));
#11922=DIRECTION('ref_axis',(0.,0.,1.));
#11923=DIRECTION('center_axis',(0.,1.,0.));
#11924=DIRECTION('ref_axis',(0.,0.,1.));
#11925=DIRECTION('center_axis',(0.,1.,0.));
#11926=DIRECTION('ref_axis',(0.,0.,1.));
#11927=DIRECTION('center_axis',(0.,1.,0.));
#11928=DIRECTION('ref_axis',(0.,0.,1.));
#11929=DIRECTION('center_axis',(0.,-1.,0.));
#11930=DIRECTION('ref_axis',(0.,0.,1.));
#11931=DIRECTION('center_axis',(0.,-1.,0.));
#11932=DIRECTION('ref_axis',(0.,0.,-1.));
#11933=DIRECTION('center_axis',(0.,0.,-1.));
#11934=DIRECTION('ref_axis',(-1.,0.,0.));
#11935=DIRECTION('center_axis',(0.,0.,1.));
#11936=DIRECTION('ref_axis',(1.,0.,0.));
#11937=DIRECTION('',(0.,0.,1.));
#11938=DIRECTION('center_axis',(0.205494612278863,0.9481117507646,-0.242602704820958));
#11939=DIRECTION('ref_axis',(6.35112393104211E-18,0.247893179847911,0.968787371606841));
#11940=DIRECTION('center_axis',(-0.205494612278863,0.9481117507646,0.242602704820958));
#11941=DIRECTION('ref_axis',(-1.40903471563721E-18,-0.247893179847911,0.968787371606841));
#11942=DIRECTION('center_axis',(0.0116178137240244,-0.999746441108087,0.0192893726178047));
#11943=DIRECTION('ref_axis',(-0.389144902110929,-0.0222903798418516,-0.920906827061012));
#11944=DIRECTION('center_axis',(0.0116178138256172,0.999746441105387,0.0192893726965582));
#11945=DIRECTION('ref_axis',(0.398644886675284,-0.022322188382412,0.916833667702856));
#11946=DIRECTION('center_axis',(-0.205494612278863,0.9481117507646,-0.242602704820958));
#11947=DIRECTION('ref_axis',(-5.52985918827002E-18,0.247893179847911,0.968787371606841));
#11948=DIRECTION('center_axis',(-0.0116178136698366,0.999746441109573,0.0192893725734215));
#11949=DIRECTION('ref_axis',(-0.389144899953581,-0.0222903797723946,0.920906827974318));
#11950=DIRECTION('center_axis',(-0.0116178138280735,-0.999746441105327,
0.0192893726981682));
#11951=DIRECTION('ref_axis',(0.398644892757021,-0.0223221884045121,-0.916833665057941));
#11952=DIRECTION('center_axis',(0.205494612278853,0.948111750764605,0.242602704820948));
#11953=DIRECTION('ref_axis',(7.91791469497955E-18,-0.247893179847899,0.968787371606844));
#11954=DIRECTION('center_axis',(0.,-1.,0.));
#11955=DIRECTION('ref_axis',(0.,0.,-1.));
#11956=DIRECTION('center_axis',(0.,-1.,0.));
#11957=DIRECTION('ref_axis',(0.,0.,-1.));
#11958=DIRECTION('',(0.,-1.,0.));
#11959=DIRECTION('center_axis',(0.,-1.,0.));
#11960=DIRECTION('ref_axis',(0.,0.,-1.));
#11961=DIRECTION('center_axis',(0.589108138320174,0.,0.80805420694712));
#11962=DIRECTION('ref_axis',(0.80805420694712,0.,-0.589108138320173));
#11963=DIRECTION('center_axis',(0.6425724926294,0.,0.766224896303977));
#11964=DIRECTION('ref_axis',(0.766224896303977,0.,-0.6425724926294));
#11965=DIRECTION('center_axis',(0.,1.,0.));
#11966=DIRECTION('ref_axis',(0.,0.,1.));
#11967=DIRECTION('center_axis',(0.642572492629448,0.,-0.766224896303936));
#11968=DIRECTION('ref_axis',(-0.766224896303936,0.,-0.642572492629448));
#11969=DIRECTION('center_axis',(0.589108138320239,0.,-0.808054206947072));
#11970=DIRECTION('ref_axis',(-0.808054206947072,0.,-0.589108138320239));
#11971=DIRECTION('center_axis',(0.589108138321627,8.53137857429337E-12,
0.80805420694606));
#11972=DIRECTION('ref_axis',(0.80805420694606,-3.6224271017081E-27,-0.589108138321627));
#11973=DIRECTION('center_axis',(0.642572492629448,0.,0.766224896303936));
#11974=DIRECTION('ref_axis',(0.766224896303936,0.,-0.642572492629448));
#11975=DIRECTION('center_axis',(0.,1.,0.));
#11976=DIRECTION('ref_axis',(0.,0.,1.));
#11977=DIRECTION('center_axis',(0.642572492629365,0.,-0.766224896304006));
#11978=DIRECTION('ref_axis',(-0.766224896304006,0.,-0.642572492629365));
#11979=DIRECTION('center_axis',(0.589108138320241,7.59621770439584E-16,
-0.808054206947071));
#11980=DIRECTION('ref_axis',(-0.808054206947071,-1.44772128095523E-31,-0.589108138320241));
#11981=DIRECTION('center_axis',(0.,0.,1.));
#11982=DIRECTION('ref_axis',(1.,0.,0.));
#11983=DIRECTION('center_axis',(0.,0.,1.));
#11984=DIRECTION('ref_axis',(1.,0.,0.));
#11985=DIRECTION('center_axis',(0.,0.,1.));
#11986=DIRECTION('ref_axis',(1.,0.,0.));
#11987=DIRECTION('center_axis',(0.,0.,-1.));
#11988=DIRECTION('ref_axis',(1.,0.,0.));
#11989=DIRECTION('',(0.,0.,-1.));
#11990=DIRECTION('center_axis',(0.,0.,1.));
#11991=DIRECTION('ref_axis',(1.,0.,0.));
#11992=DIRECTION('center_axis',(1.22464679914735E-16,-1.,0.));
#11993=DIRECTION('ref_axis',(-1.,-1.22464679914735E-16,0.));
#11994=DIRECTION('center_axis',(0.,0.,1.));
#11995=DIRECTION('ref_axis',(1.,0.,0.));
#11996=DIRECTION('center_axis',(0.,0.,1.));
#11997=DIRECTION('ref_axis',(1.,0.,0.));
#11998=DIRECTION('',(0.0195766671631255,2.39745027792948E-18,-0.999808358688196));
#11999=DIRECTION('center_axis',(0.,0.,1.));
#12000=DIRECTION('ref_axis',(1.,0.,0.));
#12001=DIRECTION('center_axis',(0.,0.,1.));
#12002=DIRECTION('ref_axis',(1.,0.,0.));
#12003=DIRECTION('center_axis',(-1.22464679914735E-16,1.,0.));
#12004=DIRECTION('ref_axis',(-1.,-1.22464679914735E-16,0.));
#12005=DIRECTION('center_axis',(0.,1.,0.));
#12006=DIRECTION('ref_axis',(0.,0.,1.));
#12007=DIRECTION('',(0.,1.,0.));
#12008=DIRECTION('center_axis',(0.,0.,1.));
#12009=DIRECTION('ref_axis',(1.,0.,0.));
#12010=DIRECTION('',(-1.,1.22163625068789E-16,0.));
#12011=DIRECTION('',(0.,-1.,0.));
#12012=DIRECTION('',(1.,-1.22163625068789E-16,0.));
#12013=DIRECTION('',(0.,1.,0.));
#12014=DIRECTION('center_axis',(-0.981627183447664,0.,-0.190808995376545));
#12015=DIRECTION('ref_axis',(0.190808995376545,0.,-0.981627183447664));
#12016=DIRECTION('',(0.190808995376545,-2.33099185709326E-17,-0.981627183447664));
#12017=DIRECTION('',(0.,-1.,0.));
#12018=DIRECTION('',(0.190808995376545,-2.33099185709326E-17,-0.981627183447664));
#12019=DIRECTION('center_axis',(1.22163625068789E-16,1.,0.));
#12020=DIRECTION('ref_axis',(-1.,1.22163625068789E-16,0.));
#12021=DIRECTION('',(1.,-1.22163625068789E-16,0.));
#12022=DIRECTION('',(-0.190808995376545,2.33099185709326E-17,-0.981627183447664));
#12023=DIRECTION('center_axis',(0.981627183447664,0.,-0.190808995376545));
#12024=DIRECTION('ref_axis',(-0.190808995376545,0.,-0.981627183447664));
#12025=DIRECTION('',(0.,1.,0.));
#12026=DIRECTION('',(-0.190808995376545,2.33099185709326E-17,-0.981627183447664));
#12027=DIRECTION('center_axis',(-1.22163625068789E-16,-1.,0.));
#12028=DIRECTION('ref_axis',(1.,-1.22163625068789E-16,0.));
#12029=DIRECTION('',(-1.,1.22163625068789E-16,0.));
#12030=DIRECTION('center_axis',(0.,0.,-1.));
#12031=DIRECTION('ref_axis',(-1.,0.,0.));
#12032=DIRECTION('axis',(0.,0.,1.));
#12033=DIRECTION('refdir',(1.,0.,0.));
#12034=DIRECTION('axis',(0.,0.,1.));
#12035=DIRECTION('refdir',(1.,0.,0.));
#12036=DIRECTION('center_axis',(-7.74415657941891E-17,0.,-1.));
#12037=DIRECTION('ref_axis',(-1.,0.,7.74415657941892E-17));
#12038=DIRECTION('',(0.,1.,0.));
#12039=DIRECTION('',(-1.,0.,7.74415657941891E-17));
#12040=DIRECTION('',(0.,1.,0.));
#12041=DIRECTION('center_axis',(0.707106781186548,0.,-0.707106781186547));
#12042=DIRECTION('ref_axis',(-0.707106781186547,0.,-0.707106781186548));
#12043=DIRECTION('',(-0.707106781186547,0.,-0.707106781186548));
#12044=DIRECTION('',(0.,1.,0.));
#12045=DIRECTION('center_axis',(1.,0.,-7.74415657941891E-17));
#12046=DIRECTION('ref_axis',(-7.74415657941891E-17,0.,-1.));
#12047=DIRECTION('',(-7.74415657941891E-17,0.,-1.));
#12048=DIRECTION('',(0.,1.,0.));
#12049=DIRECTION('center_axis',(0.707106781186547,0.,0.707106781186548));
#12050=DIRECTION('ref_axis',(0.707106781186548,0.,-0.707106781186547));
#12051=DIRECTION('',(0.707106781186548,0.,-0.707106781186547));
#12052=DIRECTION('',(0.,1.,0.));
#12053=DIRECTION('center_axis',(0.,0.,1.));
#12054=DIRECTION('ref_axis',(1.,0.,0.));
#12055=DIRECTION('',(1.,0.,0.));
#12056=DIRECTION('',(0.,1.,0.));
#12057=DIRECTION('center_axis',(-0.707106781186547,0.,0.707106781186548));
#12058=DIRECTION('ref_axis',(0.707106781186548,0.,0.707106781186547));
#12059=DIRECTION('',(0.707106781186548,0.,0.707106781186547));
#12060=DIRECTION('',(0.,1.,0.));
#12061=DIRECTION('center_axis',(-1.,0.,0.));
#12062=DIRECTION('ref_axis',(0.,0.,1.));
#12063=DIRECTION('',(0.,0.,1.));
#12064=DIRECTION('',(0.,1.,0.));
#12065=DIRECTION('center_axis',(1.,0.,1.36592399683213E-16));
#12066=DIRECTION('ref_axis',(1.36592399683213E-16,0.,-1.));
#12067=DIRECTION('center_axis',(-0.707106781186547,0.,-0.707106781186548));
#12068=DIRECTION('ref_axis',(-0.707106781186548,0.,0.707106781186547));
#12069=DIRECTION('',(-0.707106781186548,0.,0.707106781186547));
#12070=DIRECTION('center_axis',(0.,-1.,0.));
#12071=DIRECTION('ref_axis',(0.,0.,-1.));
#12072=DIRECTION('center_axis',(0.,1.,0.));
#12073=DIRECTION('ref_axis',(0.,0.,1.));
#12074=DIRECTION('',(0.,1.,0.));
#12075=DIRECTION('',(0.,-1.,0.));
#12076=DIRECTION('',(0.,1.,0.));
#12077=DIRECTION('center_axis',(0.,-1.,0.));
#12078=DIRECTION('ref_axis',(0.,0.,-1.));
#12079=DIRECTION('center_axis',(1.9436677601981E-16,-1.,0.));
#12080=DIRECTION('ref_axis',(-1.,-1.9436677601981E-16,0.));
#12081=DIRECTION('',(0.,1.,0.));
#12082=DIRECTION('center_axis',(-9.71833880099051E-17,1.,0.));
#12083=DIRECTION('ref_axis',(1.,9.71833880099051E-17,0.));
#12084=DIRECTION('center_axis',(0.,1.,0.));
#12085=DIRECTION('ref_axis',(0.,0.,1.));
#12086=DIRECTION('center_axis',(0.,-1.,0.));
#12087=DIRECTION('ref_axis',(0.,0.,-1.));
#12088=DIRECTION('center_axis',(0.,1.,0.));
#12089=DIRECTION('ref_axis',(0.,0.,1.));
#12090=DIRECTION('center_axis',(0.,-1.,0.));
#12091=DIRECTION('ref_axis',(0.,0.,-1.));
#12092=DIRECTION('center_axis',(0.,1.,0.));
#12093=DIRECTION('ref_axis',(0.,0.,-1.));
#12094=DIRECTION('',(0.,1.,0.));
#12095=DIRECTION('center_axis',(0.,1.,0.));
#12096=DIRECTION('ref_axis',(0.,0.,-1.));
#12097=DIRECTION('center_axis',(0.,-1.,0.));
#12098=DIRECTION('ref_axis',(0.,0.,-1.));
#12099=DIRECTION('center_axis',(0.,-1.,0.));
#12100=DIRECTION('ref_axis',(0.,0.,-1.));
#12101=DIRECTION('center_axis',(0.,1.,0.));
#12102=DIRECTION('ref_axis',(0.,0.,1.));
#12103=DIRECTION('center_axis',(0.,1.,0.));
#12104=DIRECTION('ref_axis',(0.,0.,1.));
#12105=DIRECTION('',(0.,1.,0.));
#12106=DIRECTION('center_axis',(0.,1.,0.));
#12107=DIRECTION('ref_axis',(0.,0.,1.));
#12108=DIRECTION('center_axis',(0.,-1.,0.));
#12109=DIRECTION('ref_axis',(0.,0.,1.));
#12110=DIRECTION('center_axis',(0.,1.,0.));
#12111=DIRECTION('ref_axis',(0.,0.,1.));
#12112=DIRECTION('center_axis',(0.,1.,0.));
#12113=DIRECTION('ref_axis',(0.,0.,1.));
#12114=DIRECTION('center_axis',(0.,1.,0.));
#12115=DIRECTION('ref_axis',(0.,0.,1.));
#12116=DIRECTION('center_axis',(0.,1.,0.));
#12117=DIRECTION('ref_axis',(0.,0.,1.));
#12118=DIRECTION('center_axis',(0.,1.,0.));
#12119=DIRECTION('ref_axis',(0.,0.,1.));
#12120=DIRECTION('center_axis',(0.,1.,0.));
#12121=DIRECTION('ref_axis',(0.,0.,1.));
#12122=DIRECTION('',(0.,-1.,0.));
#12123=DIRECTION('center_axis',(0.,-1.,0.));
#12124=DIRECTION('ref_axis',(0.,0.,-1.));
#12125=DIRECTION('center_axis',(0.,-1.,0.));
#12126=DIRECTION('ref_axis',(0.,0.,-1.));
#12127=DIRECTION('center_axis',(0.,-1.,0.));
#12128=DIRECTION('ref_axis',(0.,0.,-1.));
#12129=DIRECTION('center_axis',(0.,-1.,0.));
#12130=DIRECTION('ref_axis',(0.,0.,-1.));
#12131=DIRECTION('',(0.,1.,0.));
#12132=DIRECTION('center_axis',(0.,1.,0.));
#12133=DIRECTION('ref_axis',(0.,0.,1.));
#12134=DIRECTION('center_axis',(1.9436677601981E-16,-1.,0.));
#12135=DIRECTION('ref_axis',(-1.,-1.9436677601981E-16,0.));
#12136=DIRECTION('',(0.,1.,0.));
#12137=DIRECTION('center_axis',(0.,1.,0.));
#12138=DIRECTION('ref_axis',(0.,0.,1.));
#12139=DIRECTION('center_axis',(0.,1.,0.));
#12140=DIRECTION('ref_axis',(0.,0.,1.));
#12141=DIRECTION('',(0.,1.,0.));
#12142=DIRECTION('',(0.,1.,0.));
#12143=DIRECTION('',(0.,1.,0.));
#12144=DIRECTION('center_axis',(0.,1.,0.));
#12145=DIRECTION('ref_axis',(0.,0.,1.));
#12146=DIRECTION('center_axis',(1.9436677601981E-16,-1.,0.));
#12147=DIRECTION('ref_axis',(-1.,-1.9436677601981E-16,0.));
#12148=DIRECTION('',(0.,-1.,0.));
#12149=DIRECTION('center_axis',(-9.71833880099051E-17,1.,0.));
#12150=DIRECTION('ref_axis',(1.,9.71833880099052E-17,0.));
#12151=DIRECTION('center_axis',(0.,1.,0.));
#12152=DIRECTION('ref_axis',(0.,0.,1.));
#12153=DIRECTION('center_axis',(9.71833880099051E-17,-1.,0.));
#12154=DIRECTION('ref_axis',(1.,9.71833880099052E-17,0.));
#12155=DIRECTION('',(0.,0.,1.));
#12156=DIRECTION('',(0.,0.,1.));
#12157=DIRECTION('center_axis',(-9.71833880099051E-17,1.,0.));
#12158=DIRECTION('ref_axis',(1.,9.71833880099052E-17,0.));
#12159=DIRECTION('center_axis',(-1.,-8.41343455666662E-18,0.));
#12160=DIRECTION('ref_axis',(8.41343455666662E-18,-1.,0.));
#12161=DIRECTION('',(0.,0.,1.));
#12162=DIRECTION('center_axis',(-1.,-8.41343455666662E-18,0.));
#12163=DIRECTION('ref_axis',(8.41343455666662E-18,-1.,0.));
#12164=DIRECTION('',(0.,0.,1.));
#12165=DIRECTION('center_axis',(-1.9436677601981E-16,1.,0.));
#12166=DIRECTION('ref_axis',(-1.,-1.9436677601981E-16,0.));
#12167=DIRECTION('center_axis',(0.,1.,0.));
#12168=DIRECTION('ref_axis',(0.,0.,1.));
#12169=DIRECTION('center_axis',(0.,1.,0.));
#12170=DIRECTION('ref_axis',(0.,0.,1.));
#12171=DIRECTION('center_axis',(0.,1.,0.));
#12172=DIRECTION('ref_axis',(0.,0.,1.));
#12173=DIRECTION('',(0.,1.,0.));
#12174=DIRECTION('center_axis',(1.,0.,1.36592399683213E-16));
#12175=DIRECTION('ref_axis',(1.36592399683213E-16,0.,-1.));
#12176=DIRECTION('center_axis',(1.,0.,1.36592399683213E-16));
#12177=DIRECTION('ref_axis',(1.36592399683213E-16,0.,-1.));
#12178=DIRECTION('',(1.,0.,1.36592399683213E-16));
#12179=DIRECTION('center_axis',(1.,0.,1.36592399683213E-16));
#12180=DIRECTION('ref_axis',(1.36592399683213E-16,0.,-1.));
#12181=DIRECTION('center_axis',(0.,1.,0.));
#12182=DIRECTION('ref_axis',(0.,0.,1.));
#12183=DIRECTION('',(1.10990693043676E-16,-0.422618261740693,0.906307787036653));
#12184=DIRECTION('center_axis',(0.,-1.,0.));
#12185=DIRECTION('ref_axis',(0.,0.,-1.));
#12186=DIRECTION('center_axis',(0.,1.,0.));
#12187=DIRECTION('ref_axis',(0.,0.,1.));
#12188=DIRECTION('center_axis',(0.,1.,0.));
#12189=DIRECTION('ref_axis',(0.,0.,1.));
#12190=DIRECTION('',(8.65956056235481E-17,-0.707106781186557,0.707106781186538));
#12191=DIRECTION('center_axis',(0.,1.,0.));
#12192=DIRECTION('ref_axis',(0.,0.,1.));
#12193=DIRECTION('',(-8.65956056235497E-17,0.707106781186544,-0.707106781186551));
#12194=DIRECTION('axis',(0.,0.,1.));
#12195=DIRECTION('refdir',(1.,0.,0.));
#12196=DIRECTION('center_axis',(0.,-1.,0.));
#12197=DIRECTION('ref_axis',(0.,0.,-1.));
#12198=DIRECTION('',(0.,-1.,0.));
#12199=DIRECTION('center_axis',(0.,1.,0.));
#12200=DIRECTION('ref_axis',(0.,0.,1.));
#12201=DIRECTION('',(0.,-1.,0.));
#12202=DIRECTION('center_axis',(0.,1.,0.));
#12203=DIRECTION('ref_axis',(0.,0.,1.));
#12204=DIRECTION('center_axis',(0.,-1.,0.));
#12205=DIRECTION('ref_axis',(0.,0.,-1.));
#12206=DIRECTION('center_axis',(0.,1.,0.));
#12207=DIRECTION('ref_axis',(0.,0.,1.));
#12208=DIRECTION('',(0.,-1.,0.));
#12209=DIRECTION('center_axis',(0.,1.,0.));
#12210=DIRECTION('ref_axis',(0.,0.,1.));
#12211=DIRECTION('',(0.,-1.,0.));
#12212=DIRECTION('center_axis',(-0.158158067254484,0.,-0.987413806750912));
#12213=DIRECTION('ref_axis',(-0.987413806750912,0.,0.158158067254484));
#12214=DIRECTION('',(0.987413806750912,0.,-0.158158067254484));
#12215=DIRECTION('',(0.,-1.,0.));
#12216=DIRECTION('',(0.987413806750912,0.,-0.158158067254484));
#12217=DIRECTION('center_axis',(0.158158067254484,0.,-0.987413806750912));
#12218=DIRECTION('ref_axis',(-0.987413806750912,0.,-0.158158067254484));
#12219=DIRECTION('',(0.987413806750912,0.,0.158158067254484));
#12220=DIRECTION('',(0.987413806750912,0.,0.158158067254484));
#12221=DIRECTION('',(0.,-1.,0.));
#12222=DIRECTION('center_axis',(0.,1.,0.));
#12223=DIRECTION('ref_axis',(0.,0.,1.));
#12224=DIRECTION('',(0.392864972480271,0.,-0.919596168651259));
#12225=DIRECTION('',(-0.971825883503931,0.,-0.235699919711066));
#12226=DIRECTION('',(0.238761369565624,0.,-0.971078270997321));
#12227=DIRECTION('',(-0.997167509069151,0.,-0.0752127572744475));
#12228=DIRECTION('',(0.0783548658721971,0.,-0.996925531318237));
#12229=DIRECTION('',(-0.996185580363772,0.,0.0872598961453321));
#12230=DIRECTION('',(-0.0841200752155391,0.,-0.996455625176421));
#12231=DIRECTION('',(-0.968906018663139,0.,0.247429034267092));
#12232=DIRECTION('',(0.968906018663139,0.,0.247429034267092));
#12233=DIRECTION('',(0.0841200752155391,0.,-0.996455625176421));
#12234=DIRECTION('',(0.996185580363772,0.,0.0872598961453321));
#12235=DIRECTION('',(-0.0783548658721971,0.,-0.996925531318237));
#12236=DIRECTION('',(0.997167509069151,0.,-0.0752127572744475));
#12237=DIRECTION('',(-0.238761369565624,0.,-0.971078270997321));
#12238=DIRECTION('',(0.971825883503931,0.,-0.235699919711066));
#12239=DIRECTION('',(-0.392864972480271,0.,-0.919596168651259));
#12240=DIRECTION('center_axis',(0.,-1.,0.));
#12241=DIRECTION('ref_axis',(0.,0.,1.));
#12242=DIRECTION('center_axis',(0.,1.,0.));
#12243=DIRECTION('ref_axis',(0.,0.,1.));
#12244=DIRECTION('',(-0.392864972480271,0.,-0.919596168651259));
#12245=DIRECTION('',(0.971825883503931,0.,-0.235699919711066));
#12246=DIRECTION('',(-0.238761369565624,0.,-0.971078270997321));
#12247=DIRECTION('',(0.997167509069151,0.,-0.0752127572744475));
#12248=DIRECTION('',(-0.0783548658721971,0.,-0.996925531318237));
#12249=DIRECTION('',(0.996185580363772,0.,0.0872598961453321));
#12250=DIRECTION('',(0.0841200752155391,0.,-0.996455625176421));
#12251=DIRECTION('',(0.968906018663139,0.,0.247429034267092));
#12252=DIRECTION('',(-0.968906018663139,0.,0.247429034267092));
#12253=DIRECTION('',(-0.0841200752155391,0.,-0.996455625176421));
#12254=DIRECTION('',(-0.996185580363772,0.,0.0872598961453321));
#12255=DIRECTION('',(0.0783548658721971,0.,-0.996925531318237));
#12256=DIRECTION('',(-0.997167509069151,0.,-0.0752127572744475));
#12257=DIRECTION('',(0.238761369565624,0.,-0.971078270997321));
#12258=DIRECTION('',(-0.971825883503931,0.,-0.235699919711066));
#12259=DIRECTION('',(0.392864972480271,0.,-0.919596168651259));
#12260=DIRECTION('center_axis',(0.,1.,0.));
#12261=DIRECTION('ref_axis',(0.,0.,1.));
#12262=DIRECTION('center_axis',(0.,1.,0.));
#12263=DIRECTION('ref_axis',(0.,0.,1.));
#12264=DIRECTION('center_axis',(0.,-1.,0.));
#12265=DIRECTION('ref_axis',(0.,0.,1.));
#12266=DIRECTION('',(0.,1.,0.));
#12267=DIRECTION('center_axis',(0.,1.,0.));
#12268=DIRECTION('ref_axis',(0.,0.,1.));
#12269=DIRECTION('center_axis',(0.,-1.,0.));
#12270=DIRECTION('ref_axis',(0.,0.,1.));
#12271=DIRECTION('center_axis',(-0.91959616865126,0.,0.392864972480271));
#12272=DIRECTION('ref_axis',(0.392864972480271,0.,0.91959616865126));
#12273=DIRECTION('',(0.,-1.,0.));
#12274=DIRECTION('center_axis',(-0.235699919711066,0.,-0.971825883503932));
#12275=DIRECTION('ref_axis',(-0.971825883503932,0.,0.235699919711066));
#12276=DIRECTION('',(0.,-1.,0.));
#12277=DIRECTION('center_axis',(-0.971078270997322,0.,0.238761369565624));
#12278=DIRECTION('ref_axis',(0.238761369565624,0.,0.971078270997322));
#12279=DIRECTION('',(0.,-1.,0.));
#12280=DIRECTION('center_axis',(-0.0752127572744475,0.,-0.997167509069151));
#12281=DIRECTION('ref_axis',(-0.997167509069151,0.,0.0752127572744475));
#12282=DIRECTION('',(0.,-1.,0.));
#12283=DIRECTION('center_axis',(-0.996925531318237,0.,0.0783548658721971));
#12284=DIRECTION('ref_axis',(0.0783548658721971,0.,0.996925531318237));
#12285=DIRECTION('',(0.,-1.,0.));
#12286=DIRECTION('center_axis',(0.0872598961453321,0.,-0.996185580363772));
#12287=DIRECTION('ref_axis',(-0.996185580363772,0.,-0.0872598961453321));
#12288=DIRECTION('',(0.,-1.,0.));
#12289=DIRECTION('center_axis',(-0.996455625176421,0.,-0.0841200752155391));
#12290=DIRECTION('ref_axis',(-0.0841200752155391,0.,0.996455625176421));
#12291=DIRECTION('',(0.,-1.,0.));
#12292=DIRECTION('center_axis',(0.247429034267092,0.,-0.968906018663139));
#12293=DIRECTION('ref_axis',(-0.968906018663139,0.,-0.247429034267092));
#12294=DIRECTION('center_axis',(-0.91959616865126,0.,-0.392864972480271));
#12295=DIRECTION('ref_axis',(-0.392864972480271,0.,0.91959616865126));
#12296=DIRECTION('',(0.,-1.,0.));
#12297=DIRECTION('center_axis',(-0.235699919711066,0.,0.971825883503932));
#12298=DIRECTION('ref_axis',(0.971825883503932,0.,0.235699919711066));
#12299=DIRECTION('',(0.,-1.,0.));
#12300=DIRECTION('center_axis',(-0.971078270997322,0.,-0.238761369565624));
#12301=DIRECTION('ref_axis',(-0.238761369565624,0.,0.971078270997322));
#12302=DIRECTION('',(0.,-1.,0.));
#12303=DIRECTION('center_axis',(-0.0752127572744475,0.,0.997167509069151));
#12304=DIRECTION('ref_axis',(0.997167509069151,0.,0.0752127572744475));
#12305=DIRECTION('',(0.,-1.,0.));
#12306=DIRECTION('center_axis',(-0.996925531318237,0.,-0.0783548658721971));
#12307=DIRECTION('ref_axis',(-0.0783548658721971,0.,0.996925531318237));
#12308=DIRECTION('',(0.,-1.,0.));
#12309=DIRECTION('center_axis',(0.0872598961453321,0.,0.996185580363772));
#12310=DIRECTION('ref_axis',(0.996185580363772,0.,-0.0872598961453321));
#12311=DIRECTION('',(0.,-1.,0.));
#12312=DIRECTION('center_axis',(-0.996455625176421,0.,0.0841200752155391));
#12313=DIRECTION('ref_axis',(0.0841200752155391,0.,0.996455625176421));
#12314=DIRECTION('',(0.,-1.,0.));
#12315=DIRECTION('center_axis',(0.247429034267092,0.,0.968906018663139));
#12316=DIRECTION('ref_axis',(0.968906018663139,0.,-0.247429034267092));
#12317=DIRECTION('center_axis',(0.,-1.,0.));
#12318=DIRECTION('ref_axis',(0.,0.,-1.));
#12319=DIRECTION('',(-8.65956056235489E-17,-0.707106781186551,0.707106781186544));
#12320=DIRECTION('center_axis',(0.,1.,0.));
#12321=DIRECTION('ref_axis',(0.,0.,1.));
#12322=DIRECTION('',(-8.65956056235494E-17,0.707106781186546,-0.707106781186549));
#12323=DIRECTION('axis',(0.,0.,1.));
#12324=DIRECTION('refdir',(1.,0.,0.));
#12325=DIRECTION('center_axis',(0.,-1.,0.));
#12326=DIRECTION('ref_axis',(0.,0.,-1.));
#12327=DIRECTION('center_axis',(0.,1.,0.));
#12328=DIRECTION('ref_axis',(0.,0.,1.));
#12329=DIRECTION('center_axis',(0.,1.,0.));
#12330=DIRECTION('ref_axis',(0.,0.,1.));
#12331=DIRECTION('',(0.,1.,0.));
#12332=DIRECTION('center_axis',(0.,-1.,0.));
#12333=DIRECTION('ref_axis',(0.,0.,1.));
#12334=DIRECTION('center_axis',(0.,1.,0.));
#12335=DIRECTION('ref_axis',(0.,0.,1.));
#12336=DIRECTION('center_axis',(0.,1.,0.));
#12337=DIRECTION('ref_axis',(0.,0.,1.));
#12338=DIRECTION('center_axis',(0.,1.,0.));
#12339=DIRECTION('ref_axis',(0.,0.,1.));
#12340=DIRECTION('center_axis',(0.,-1.,0.));
#12341=DIRECTION('ref_axis',(0.,0.,1.));
#12342=DIRECTION('center_axis',(0.,1.,0.));
#12343=DIRECTION('ref_axis',(0.,0.,1.));
#12344=DIRECTION('',(8.65956056235493E-17,-0.707106781186548,0.707106781186547));
#12345=DIRECTION('center_axis',(0.,-1.,0.));
#12346=DIRECTION('ref_axis',(0.,0.,-1.));
#12347=DIRECTION('',(8.65956056235491E-17,0.707106781186549,-0.707106781186546));
#12348=DIRECTION('axis',(0.,0.,1.));
#12349=DIRECTION('refdir',(1.,0.,0.));
#12350=DIRECTION('center_axis',(0.,-1.,0.));
#12351=DIRECTION('ref_axis',(0.,0.,-1.));
#12352=DIRECTION('center_axis',(0.,-1.,0.));
#12353=DIRECTION('ref_axis',(0.,0.,-1.));
#12354=DIRECTION('center_axis',(0.,-1.,0.));
#12355=DIRECTION('ref_axis',(0.,0.,-1.));
#12356=DIRECTION('center_axis',(0.,1.,0.));
#12357=DIRECTION('ref_axis',(0.,0.,-1.));
#12358=DIRECTION('',(0.,1.,0.));
#12359=DIRECTION('center_axis',(0.,-1.,0.));
#12360=DIRECTION('ref_axis',(0.,0.,-1.));
#12361=DIRECTION('center_axis',(0.,1.,0.));
#12362=DIRECTION('ref_axis',(0.,0.,-1.));
#12363=DIRECTION('center_axis',(0.,-1.,0.));
#12364=DIRECTION('ref_axis',(0.,0.,-1.));
#12365=DIRECTION('center_axis',(0.,-1.,0.));
#12366=DIRECTION('ref_axis',(0.,0.,-1.));
#12367=DIRECTION('center_axis',(0.,-1.,0.));
#12368=DIRECTION('ref_axis',(0.,0.,-1.));
#12369=DIRECTION('center_axis',(0.,1.,0.));
#12370=DIRECTION('ref_axis',(0.,0.,-1.));
#12371=DIRECTION('',(0.,1.,0.));
#12372=DIRECTION('center_axis',(0.,-1.,0.));
#12373=DIRECTION('ref_axis',(0.,0.,-1.));
#12374=DIRECTION('center_axis',(0.,1.,0.));
#12375=DIRECTION('ref_axis',(0.,0.,-1.));
#12376=DIRECTION('center_axis',(0.,1.,0.));
#12377=DIRECTION('ref_axis',(0.,0.,1.));
#12378=DIRECTION('center_axis',(0.,1.,0.));
#12379=DIRECTION('ref_axis',(0.,0.,1.));
#12380=DIRECTION('center_axis',(0.,-1.,0.));
#12381=DIRECTION('ref_axis',(0.,0.,1.));
#12382=DIRECTION('',(-1.,0.,0.));
#12383=DIRECTION('center_axis',(0.,-1.,0.));
#12384=DIRECTION('ref_axis',(0.,0.,1.));
#12385=DIRECTION('center_axis',(0.,1.,0.));
#12386=DIRECTION('ref_axis',(0.,0.,1.));
#12387=DIRECTION('center_axis',(0.,-1.,0.));
#12388=DIRECTION('ref_axis',(1.73472347597681E-15,0.,1.));
#12389=DIRECTION('',(1.,0.,0.));
#12390=DIRECTION('center_axis',(0.,-1.,0.));
#12391=DIRECTION('ref_axis',(0.,0.,1.));
#12392=DIRECTION('center_axis',(0.,-1.,0.));
#12393=DIRECTION('ref_axis',(0.,0.,-1.));
#12394=DIRECTION('center_axis',(0.,1.,0.));
#12395=DIRECTION('ref_axis',(0.,0.,1.));
#12396=DIRECTION('',(0.,-1.,0.));
#12397=DIRECTION('',(0.,1.,0.));
#12398=DIRECTION('center_axis',(0.,0.,-1.));
#12399=DIRECTION('ref_axis',(-1.,0.,0.));
#12400=DIRECTION('',(0.,1.,0.));
#12401=DIRECTION('',(1.,0.,0.));
#12402=DIRECTION('',(0.,-1.,0.));
#12403=DIRECTION('center_axis',(0.,-1.,0.));
#12404=DIRECTION('ref_axis',(0.,0.,-1.));
#12405=DIRECTION('',(0.,1.,0.));
#12406=DIRECTION('center_axis',(0.,1.,0.));
#12407=DIRECTION('ref_axis',(0.,0.,1.));
#12408=DIRECTION('',(0.,-1.,0.));
#12409=DIRECTION('center_axis',(0.,0.,1.));
#12410=DIRECTION('ref_axis',(1.,0.,0.));
#12411=DIRECTION('',(0.,1.,0.));
#12412=DIRECTION('',(-1.,0.,0.));
#12413=DIRECTION('',(0.,-1.,0.));
#12414=DIRECTION('center_axis',(0.,1.,0.));
#12415=DIRECTION('ref_axis',(0.,0.,1.));
#12416=DIRECTION('center_axis',(0.,1.,0.));
#12417=DIRECTION('ref_axis',(0.,0.,1.));
#12418=DIRECTION('center_axis',(0.,1.,0.));
#12419=DIRECTION('ref_axis',(0.,0.,1.));
#12420=DIRECTION('center_axis',(0.,1.,0.));
#12421=DIRECTION('ref_axis',(0.,0.,1.));
#12422=DIRECTION('center_axis',(0.,1.,0.));
#12423=DIRECTION('ref_axis',(0.,0.,1.));
#12424=DIRECTION('center_axis',(1.,0.,0.));
#12425=DIRECTION('ref_axis',(0.,0.,-1.));
#12426=DIRECTION('center_axis',(1.,0.,0.));
#12427=DIRECTION('ref_axis',(0.,0.,-1.));
#12428=DIRECTION('',(1.,0.,0.));
#12429=DIRECTION('center_axis',(1.,0.,0.));
#12430=DIRECTION('ref_axis',(0.,0.,-1.));
#12431=DIRECTION('center_axis',(0.,1.,0.));
#12432=DIRECTION('ref_axis',(0.,0.,1.));
#12433=DIRECTION('',(8.6595605623549E-17,-0.70710678118655,0.707106781186545));
#12434=DIRECTION('center_axis',(0.,1.,0.));
#12435=DIRECTION('ref_axis',(0.,0.,1.));
#12436=DIRECTION('',(8.65956056235492E-17,-0.707106781186549,0.707106781186546));
#12437=DIRECTION('center_axis',(0.,-1.,0.));
#12438=DIRECTION('ref_axis',(0.,0.,-1.));
#12439=DIRECTION('center_axis',(0.,-1.,0.));
#12440=DIRECTION('ref_axis',(0.,0.,-1.));
#12441=DIRECTION('center_axis',(0.,-1.,0.));
#12442=DIRECTION('ref_axis',(0.,0.,-1.));
#12443=DIRECTION('center_axis',(0.,-1.,0.));
#12444=DIRECTION('ref_axis',(0.,0.,-1.));
#12445=DIRECTION('axis',(0.,0.,1.));
#12446=DIRECTION('refdir',(1.,0.,0.));
#12447=DIRECTION('center_axis',(1.,0.,8.37955521322352E-14));
#12448=DIRECTION('ref_axis',(8.37955521322352E-14,0.,-1.));
#12449=DIRECTION('center_axis',(1.,0.,0.));
#12450=DIRECTION('ref_axis',(0.,0.,-1.));
#12451=DIRECTION('center_axis',(1.,0.,0.));
#12452=DIRECTION('ref_axis',(0.,0.,-1.));
#12453=DIRECTION('center_axis',(1.,0.,8.37955521322352E-14));
#12454=DIRECTION('ref_axis',(8.37955521322352E-14,0.,-1.));
#12455=DIRECTION('center_axis',(1.,0.,0.));
#12456=DIRECTION('ref_axis',(0.,0.,-1.));
#12457=DIRECTION('center_axis',(1.,0.,8.37955521322352E-14));
#12458=DIRECTION('ref_axis',(8.37955521322352E-14,0.,-1.));
#12459=DIRECTION('center_axis',(1.,0.,0.));
#12460=DIRECTION('ref_axis',(0.,0.,-1.));
#12461=DIRECTION('center_axis',(1.,0.,8.37955521322352E-14));
#12462=DIRECTION('ref_axis',(8.37955521322352E-14,0.,-1.));
#12463=DIRECTION('center_axis',(1.,0.,8.37955521322352E-14));
#12464=DIRECTION('ref_axis',(8.37955521322352E-14,0.,-1.));
#12465=DIRECTION('center_axis',(1.,0.,0.));
#12466=DIRECTION('ref_axis',(0.,0.,-1.));
#12467=DIRECTION('axis',(0.,0.,1.));
#12468=DIRECTION('refdir',(1.,0.,0.));
#12469=DIRECTION('center_axis',(1.,0.,8.37955521322352E-14));
#12470=DIRECTION('ref_axis',(8.37955521322352E-14,0.,-1.));
#12471=DIRECTION('center_axis',(1.,0.,0.));
#12472=DIRECTION('ref_axis',(0.,0.,-1.));
#12473=DIRECTION('center_axis',(1.,0.,0.));
#12474=DIRECTION('ref_axis',(0.,0.,-1.));
#12475=DIRECTION('center_axis',(1.,0.,8.37955521322352E-14));
#12476=DIRECTION('ref_axis',(8.37955521322352E-14,0.,-1.));
#12477=DIRECTION('center_axis',(1.,0.,0.));
#12478=DIRECTION('ref_axis',(0.,0.,-1.));
#12479=DIRECTION('center_axis',(1.,0.,8.37955521322352E-14));
#12480=DIRECTION('ref_axis',(8.37955521322352E-14,0.,-1.));
#12481=DIRECTION('center_axis',(1.,0.,0.));
#12482=DIRECTION('ref_axis',(0.,0.,-1.));
#12483=DIRECTION('center_axis',(1.,0.,8.37955521322352E-14));
#12484=DIRECTION('ref_axis',(8.37955521322352E-14,0.,-1.));
#12485=DIRECTION('center_axis',(1.,0.,8.37955521322352E-14));
#12486=DIRECTION('ref_axis',(8.37955521322352E-14,0.,-1.));
#12487=DIRECTION('center_axis',(1.,0.,0.));
#12488=DIRECTION('ref_axis',(0.,0.,-1.));
#12489=DIRECTION('axis',(0.,0.,1.));
#12490=DIRECTION('refdir',(1.,0.,0.));
#12491=DIRECTION('center_axis',(-1.,5.55111512312579E-17,6.12323399573673E-17));
#12492=DIRECTION('ref_axis',(-4.07638157631888E-31,2.09541177949331E-31,
1.));
#12493=DIRECTION('center_axis',(-5.55111512312579E-17,-1.,1.22464679914736E-16));
#12494=DIRECTION('ref_axis',(4.00840002264653E-31,-1.22464679914736E-16,
-1.));
#12495=DIRECTION('',(0.,0.,1.));
#12496=DIRECTION('',(1.,0.,0.));
#12497=DIRECTION('',(-0.984807753012213,1.72256092499685E-17,0.173648177666903));
#12498=DIRECTION('',(0.173648177666903,-7.72233180999998E-17,0.984807753012213));
#12499=DIRECTION('',(0.,0.,1.));
#12500=DIRECTION('',(1.,0.,0.));
#12501=DIRECTION('',(0.,0.,1.));
#12502=DIRECTION('',(1.,0.,0.));
#12503=DIRECTION('',(-6.98296267768627E-15,-2.43808838789797E-29,-1.));
#12504=DIRECTION('',(-3.49148133884313E-15,1.,0.));
#12505=DIRECTION('',(1.,3.52642466643932E-15,0.));
#12506=DIRECTION('',(4.13909153814718E-31,-1.17373598748289E-16,1.));
#12507=DIRECTION('',(0.,0.,1.));
#12508=DIRECTION('',(-3.49148133884313E-15,1.,0.));
#12509=DIRECTION('',(3.50731635025523E-15,-1.,3.96548102751435E-17));
#12510=DIRECTION('',(-1.,-3.50731635025523E-15,-3.33066907387547E-16));
#12511=DIRECTION('axis',(0.,0.,1.));
#12512=DIRECTION('refdir',(1.,0.,0.));
#12513=DIRECTION('center_axis',(0.,1.,0.));
#12514=DIRECTION('ref_axis',(0.,0.,1.));
#12515=DIRECTION('center_axis',(-1.,0.,1.22464679914735E-16));
#12516=DIRECTION('ref_axis',(-1.22464679914735E-16,0.,-1.));
#12517=DIRECTION('center_axis',(0.,-1.,0.));
#12518=DIRECTION('ref_axis',(0.,0.,1.));
#12519=DIRECTION('axis',(0.,0.,1.));
#12520=DIRECTION('refdir',(1.,0.,0.));
#12521=DIRECTION('axis',(0.,0.,1.));
#12522=DIRECTION('refdir',(1.,0.,0.));
#12523=DIRECTION('center_axis',(0.,-1.,0.));
#12524=DIRECTION('ref_axis',(0.,0.,-1.));
#12525=DIRECTION('center_axis',(0.,-1.,0.));
#12526=DIRECTION('ref_axis',(0.,0.,-1.));
#12527=DIRECTION('',(0.,1.,0.));
#12528=DIRECTION('',(0.,-1.,-4.68844182696434E-17));
#12529=DIRECTION('',(0.,1.,0.));
#12530=DIRECTION('center_axis',(0.,1.,0.));
#12531=DIRECTION('ref_axis',(0.,0.,1.));
#12532=DIRECTION('',(0.,1.,4.68844182696434E-17));
#12533=DIRECTION('',(4.45897315080518E-17,-1.,1.44880820167036E-17));
#12534=DIRECTION('',(-4.45897315080518E-17,1.,-1.44880820167036E-17));
#12535=DIRECTION('',(2.75579696212085E-17,-1.,-3.79302911515246E-17));
#12536=DIRECTION('',(-2.75579696212085E-17,1.,3.79302911515246E-17));
#12537=DIRECTION('',(-2.7557969621208E-17,-1.,-3.7930291151525E-17));
#12538=DIRECTION('',(2.7557969621208E-17,1.,3.7930291151525E-17));
#12539=DIRECTION('',(-4.4589731508052E-17,-1.,1.4488082016703E-17));
#12540=DIRECTION('',(4.4589731508052E-17,1.,-1.4488082016703E-17));
#12541=DIRECTION('',(0.,-1.,4.68844182696434E-17));
#12542=DIRECTION('',(0.,1.,-4.68844182696434E-17));
#12543=DIRECTION('',(-2.75579696212083E-17,-1.,3.79302911515248E-17));
#12544=DIRECTION('',(2.75579696212083E-17,1.,-3.79302911515248E-17));
#12545=DIRECTION('',(-4.45897315080519E-17,-1.,-1.44880820167033E-17));
#12546=DIRECTION('',(4.45897315080519E-17,1.,1.44880820167033E-17));
#12547=DIRECTION('',(4.45897315080521E-17,-1.,-1.44880820167027E-17));
#12548=DIRECTION('',(-4.45897315080521E-17,1.,1.44880820167027E-17));
#12549=DIRECTION('',(2.75579696212077E-17,-1.,3.79302911515252E-17));
#12550=DIRECTION('',(-2.75579696212077E-17,1.,-3.79302911515252E-17));
#12551=DIRECTION('center_axis',(0.,-1.,0.));
#12552=DIRECTION('ref_axis',(0.,0.,-1.));
#12553=DIRECTION('center_axis',(0.,-1.,0.));
#12554=DIRECTION('ref_axis',(0.,0.,-1.));
#12555=DIRECTION('',(0.,1.,0.));
#12556=DIRECTION('',(0.,1.,0.));
#12557=DIRECTION('center_axis',(0.,-1.,0.));
#12558=DIRECTION('ref_axis',(0.,0.,1.));
#12559=DIRECTION('center_axis',(0.,-1.,0.));
#12560=DIRECTION('ref_axis',(0.,0.,-1.));
#12561=DIRECTION('center_axis',(0.,1.,0.));
#12562=DIRECTION('ref_axis',(0.,0.,1.));
#12563=DIRECTION('center_axis',(0.,1.,0.));
#12564=DIRECTION('ref_axis',(0.,0.,1.));
#12565=DIRECTION('',(0.,1.,0.));
#12566=DIRECTION('',(0.,1.,0.));
#12567=DIRECTION('center_axis',(0.,1.,0.));
#12568=DIRECTION('ref_axis',(0.,0.,1.));
#12569=DIRECTION('center_axis',(0.,1.,0.));
#12570=DIRECTION('ref_axis',(0.,0.,1.));
#12571=DIRECTION('center_axis',(0.,1.,0.));
#12572=DIRECTION('ref_axis',(0.,0.,1.));
#12573=DIRECTION('center_axis',(0.,-1.,0.));
#12574=DIRECTION('ref_axis',(0.,0.,1.));
#12575=DIRECTION('center_axis',(0.,1.,0.));
#12576=DIRECTION('ref_axis',(0.,0.,1.));
#12577=DIRECTION('center_axis',(0.,-1.,0.));
#12578=DIRECTION('ref_axis',(0.,0.,1.));
#12579=DIRECTION('center_axis',(0.,1.,0.));
#12580=DIRECTION('ref_axis',(0.,0.,1.));
#12581=DIRECTION('center_axis',(0.,1.,0.));
#12582=DIRECTION('ref_axis',(0.,0.,1.));
#12583=DIRECTION('center_axis',(0.,-1.,0.));
#12584=DIRECTION('ref_axis',(0.,0.,1.));
#12585=DIRECTION('',(0.,1.,0.));
#12586=DIRECTION('',(0.,1.,0.));
#12587=DIRECTION('',(0.,1.,0.));
#12588=DIRECTION('center_axis',(0.,1.,0.));
#12589=DIRECTION('ref_axis',(0.,0.,1.));
#12590=DIRECTION('center_axis',(0.,-1.,0.));
#12591=DIRECTION('ref_axis',(0.,0.,1.));
#12592=DIRECTION('center_axis',(0.,0.,1.));
#12593=DIRECTION('ref_axis',(1.,0.,0.));
#12594=DIRECTION('',(0.,0.,1.));
#12595=DIRECTION('center_axis',(0.,0.,1.));
#12596=DIRECTION('ref_axis',(1.,0.,0.));
#12597=DIRECTION('',(0.,0.,1.));
#12598=DIRECTION('center_axis',(0.,0.,1.));
#12599=DIRECTION('ref_axis',(1.,0.,0.));
#12600=DIRECTION('',(0.,0.,1.));
#12601=DIRECTION('center_axis',(0.,0.,1.));
#12602=DIRECTION('ref_axis',(1.,0.,0.));
#12603=DIRECTION('',(0.,0.,1.));
#12604=DIRECTION('center_axis',(0.,-1.,0.));
#12605=DIRECTION('ref_axis',(0.,0.,-1.));
#12606=DIRECTION('center_axis',(1.,0.,1.22464679914735E-16));
#12607=DIRECTION('ref_axis',(-1.22464679914735E-16,0.,1.));
#12608=DIRECTION('center_axis',(0.,-1.,0.));
#12609=DIRECTION('ref_axis',(0.,0.,-1.));
#12610=DIRECTION('center_axis',(1.,0.,1.22464679914735E-16));
#12611=DIRECTION('ref_axis',(-1.22464679914735E-16,0.,1.));
#12612=DIRECTION('center_axis',(0.,-1.,0.));
#12613=DIRECTION('ref_axis',(0.,0.,-1.));
#12614=DIRECTION('center_axis',(0.,1.,-4.68844182696434E-17));
#12615=DIRECTION('ref_axis',(0.,4.68844182696434E-17,1.));
#12616=DIRECTION('center_axis',(0.,-1.,0.));
#12617=DIRECTION('ref_axis',(0.,0.,-1.));
#12618=DIRECTION('center_axis',(0.,-1.,0.));
#12619=DIRECTION('ref_axis',(0.587785252292474,0.,-0.809016994374947));
#12620=DIRECTION('center_axis',(2.75579696212083E-17,1.,-3.79302911515248E-17));
#12621=DIRECTION('ref_axis',(1.0452818112773E-33,3.79302911515248E-17,1.));
#12622=DIRECTION('center_axis',(0.,-1.,0.));
#12623=DIRECTION('ref_axis',(0.587785252292474,0.,-0.809016994374947));
#12624=DIRECTION('center_axis',(0.,-1.,0.));
#12625=DIRECTION('ref_axis',(0.951056516295154,0.,-0.309016994374945));
#12626=DIRECTION('center_axis',(4.4589731508052E-17,1.,-1.4488082016703E-17));
#12627=DIRECTION('ref_axis',(-1.,4.4589731508052E-17,-6.46019687191422E-34));
#12628=DIRECTION('center_axis',(0.,-1.,0.));
#12629=DIRECTION('ref_axis',(0.951056516295155,0.,-0.309016994374944));
#12630=DIRECTION('center_axis',(0.,-1.,0.));
#12631=DIRECTION('ref_axis',(0.951056516295152,0.,0.309016994374952));
#12632=DIRECTION('center_axis',(4.45897315080519E-17,1.,1.44880820167033E-17));
#12633=DIRECTION('ref_axis',(-1.,4.45897315080519E-17,6.46019687191434E-34));
#12634=DIRECTION('center_axis',(0.,-1.,0.));
#12635=DIRECTION('ref_axis',(0.951056516295152,0.,0.309016994374952));
#12636=DIRECTION('center_axis',(0.,-1.,0.));
#12637=DIRECTION('ref_axis',(0.587785252292469,0.,0.809016994374951));
#12638=DIRECTION('center_axis',(2.7557969621208E-17,1.,3.7930291151525E-17));
#12639=DIRECTION('ref_axis',(-0.587785252292469,4.68844182696434E-17,-0.80901699437495));
#12640=DIRECTION('center_axis',(0.,-1.,0.));
#12641=DIRECTION('ref_axis',(0.587785252292469,0.,0.809016994374951));
#12642=DIRECTION('center_axis',(0.,-1.,0.));
#12643=DIRECTION('ref_axis',(0.,0.,1.));
#12644=DIRECTION('center_axis',(0.,1.,4.68844182696434E-17));
#12645=DIRECTION('ref_axis',(-1.22464679914735E-16,4.68844182696434E-17,
-1.));
#12646=DIRECTION('center_axis',(0.,-1.,0.));
#12647=DIRECTION('ref_axis',(0.,0.,1.));
#12648=DIRECTION('center_axis',(0.,-1.,0.));
#12649=DIRECTION('ref_axis',(-0.587785252292481,0.,0.809016994374942));
#12650=DIRECTION('center_axis',(-2.75579696212085E-17,1.,3.79302911515246E-17));
#12651=DIRECTION('ref_axis',(0.58778525229248,4.68844182696434E-17,-0.809016994374942));
#12652=DIRECTION('center_axis',(0.,-1.,0.));
#12653=DIRECTION('ref_axis',(-0.587785252292481,0.,0.809016994374942));
#12654=DIRECTION('center_axis',(0.,-1.,0.));
#12655=DIRECTION('ref_axis',(-0.951056516295156,0.,0.309016994374938));
#12656=DIRECTION('center_axis',(-4.45897315080521E-17,1.,1.44880820167027E-17));
#12657=DIRECTION('ref_axis',(0.951056516295156,4.68844182696434E-17,-0.309016994374939));
#12658=DIRECTION('center_axis',(0.,-1.,0.));
#12659=DIRECTION('ref_axis',(-0.951056516295156,0.,0.309016994374938));
#12660=DIRECTION('center_axis',(0.,-1.,0.));
#12661=DIRECTION('ref_axis',(-0.95105651629515,0.,-0.309016994374958));
#12662=DIRECTION('center_axis',(-4.45897315080518E-17,1.,-1.44880820167036E-17));
#12663=DIRECTION('ref_axis',(0.95105651629515,4.68844182696434E-17,0.309016994374958));
#12664=DIRECTION('center_axis',(0.,-1.,0.));
#12665=DIRECTION('ref_axis',(-0.95105651629515,0.,-0.309016994374958));
#12666=DIRECTION('center_axis',(0.,-1.,0.));
#12667=DIRECTION('ref_axis',(-0.587785252292462,0.,-0.809016994374955));
#12668=DIRECTION('center_axis',(-2.75579696212077E-17,1.,-3.79302911515252E-17));
#12669=DIRECTION('ref_axis',(-1.04528181127729E-33,3.79302911515252E-17,
1.));
#12670=DIRECTION('center_axis',(0.,-1.,0.));
#12671=DIRECTION('ref_axis',(-0.587785252292462,0.,-0.809016994374955));
#12672=DIRECTION('center_axis',(0.,1.,0.));
#12673=DIRECTION('ref_axis',(0.,0.,1.));
#12674=DIRECTION('',(-8.65956056235505E-17,0.707106781186538,-0.707106781186557));
#12675=DIRECTION('center_axis',(0.,-1.,0.));
#12676=DIRECTION('ref_axis',(0.,0.,-1.));
#12677=DIRECTION('',(-8.65956056235496E-17,-0.707106781186545,0.70710678118655));
#12678=DIRECTION('center_axis',(0.,-1.,0.));
#12679=DIRECTION('ref_axis',(0.,0.,-1.));
#12680=DIRECTION('',(8.65956056235472E-17,0.707106781186565,-0.70710678118653));
#12681=DIRECTION('center_axis',(0.,1.,0.));
#12682=DIRECTION('ref_axis',(0.,0.,1.));
#12683=DIRECTION('',(8.65956056235519E-17,-0.707106781186527,0.707106781186568));
#12684=DIRECTION('axis',(0.,0.,1.));
#12685=DIRECTION('refdir',(1.,0.,0.));
#12686=DIRECTION('center_axis',(0.,-1.,0.));
#12687=DIRECTION('ref_axis',(0.,0.,-1.));
#12688=DIRECTION('center_axis',(0.,1.,0.));
#12689=DIRECTION('ref_axis',(0.,0.,1.));
#12690=DIRECTION('',(0.,1.,0.));
#12691=DIRECTION('',(0.,1.,0.));
#12692=DIRECTION('center_axis',(0.,1.,0.));
#12693=DIRECTION('ref_axis',(0.,0.,1.));
#12694=DIRECTION('center_axis',(0.,1.,0.));
#12695=DIRECTION('ref_axis',(0.,0.,1.));
#12696=DIRECTION('center_axis',(0.,1.,0.));
#12697=DIRECTION('ref_axis',(0.,0.,1.));
#12698=DIRECTION('center_axis',(0.,1.,0.));
#12699=DIRECTION('ref_axis',(0.,0.,1.));
#12700=DIRECTION('center_axis',(0.,-1.,0.));
#12701=DIRECTION('ref_axis',(0.,0.,-1.));
#12702=DIRECTION('center_axis',(0.,0.,1.));
#12703=DIRECTION('ref_axis',(1.,0.,0.));
#12704=DIRECTION('center_axis',(0.,0.,1.));
#12705=DIRECTION('ref_axis',(1.,0.,0.));
#12706=DIRECTION('',(0.,0.,1.));
#12707=DIRECTION('center_axis',(0.,0.,1.));
#12708=DIRECTION('ref_axis',(1.,0.,0.));
#12709=DIRECTION('center_axis',(0.,0.,-1.));
#12710=DIRECTION('ref_axis',(-1.,0.,0.));
#12711=DIRECTION('center_axis',(0.,0.,1.));
#12712=DIRECTION('ref_axis',(1.,0.,0.));
#12713=DIRECTION('',(0.,0.,-1.));
#12714=DIRECTION('center_axis',(0.,0.,-1.));
#12715=DIRECTION('ref_axis',(1.,0.,0.));
#12716=DIRECTION('center_axis',(0.,-1.,0.));
#12717=DIRECTION('ref_axis',(0.,0.,-1.));
#12718=DIRECTION('',(0.,-1.,0.));
#12719=DIRECTION('axis',(0.,0.,1.));
#12720=DIRECTION('refdir',(1.,0.,0.));
#12721=DIRECTION('center_axis',(0.,1.,0.));
#12722=DIRECTION('ref_axis',(0.,0.,1.));
#12723=DIRECTION('center_axis',(0.,-1.,0.));
#12724=DIRECTION('ref_axis',(0.,0.,-1.));
#12725=DIRECTION('center_axis',(0.,1.,0.));
#12726=DIRECTION('ref_axis',(0.,0.,1.));
#12727=DIRECTION('center_axis',(0.,-1.,0.));
#12728=DIRECTION('ref_axis',(0.,0.,-1.));
#12729=DIRECTION('',(0.,1.,0.));
#12730=DIRECTION('center_axis',(0.,-1.,0.));
#12731=DIRECTION('ref_axis',(0.,0.,-1.));
#12732=DIRECTION('center_axis',(0.,-1.,0.));
#12733=DIRECTION('ref_axis',(0.,0.,-1.));
#12734=DIRECTION('center_axis',(0.,1.,0.));
#12735=DIRECTION('ref_axis',(0.,0.,-1.));
#12736=DIRECTION('center_axis',(0.,-1.,0.));
#12737=DIRECTION('ref_axis',(0.,0.,-1.));
#12738=DIRECTION('center_axis',(0.,1.,-6.12323399573677E-17));
#12739=DIRECTION('ref_axis',(0.,0.,-1.));
#12740=DIRECTION('center_axis',(1.,0.,-1.22464679914735E-16));
#12741=DIRECTION('ref_axis',(1.22464679914735E-16,0.,1.));
#12742=DIRECTION('center_axis',(0.,-1.,0.));
#12743=DIRECTION('ref_axis',(0.,0.,-1.));
#12744=DIRECTION('center_axis',(-1.,0.,-1.22464679914735E-16));
#12745=DIRECTION('ref_axis',(-1.22464679914735E-16,0.,1.));
#12746=DIRECTION('center_axis',(0.,1.,0.));
#12747=DIRECTION('ref_axis',(0.,0.,1.));
#12748=DIRECTION('',(0.,-1.,0.));
#12749=DIRECTION('center_axis',(0.,1.,0.));
#12750=DIRECTION('ref_axis',(0.,0.,1.));
#12751=DIRECTION('center_axis',(0.,1.,0.));
#12752=DIRECTION('ref_axis',(0.,0.,1.));
#12753=DIRECTION('',(8.65956056235499E-17,-0.707106781186542,0.707106781186553));
#12754=DIRECTION('center_axis',(0.,1.,0.));
#12755=DIRECTION('ref_axis',(0.,0.,1.));
#12756=DIRECTION('center_axis',(0.,-1.,0.));
#12757=DIRECTION('ref_axis',(0.,0.,-1.));
#12758=DIRECTION('',(-0.866025403784438,0.,0.5));
#12759=DIRECTION('',(-0.866025403784439,0.,-0.5));
#12760=DIRECTION('',(0.,0.,-1.));
#12761=DIRECTION('',(0.866025403784438,0.,-0.5));
#12762=DIRECTION('',(0.866025403784439,0.,0.5));
#12763=DIRECTION('',(0.,0.,1.));
#12764=DIRECTION('center_axis',(-1.,0.,0.));
#12765=DIRECTION('ref_axis',(0.,0.,1.));
#12766=DIRECTION('',(0.,0.,-1.));
#12767=DIRECTION('',(0.,-1.,0.));
#12768=DIRECTION('',(0.,-1.,0.));
#12769=DIRECTION('center_axis',(-0.5,0.,-0.866025403784439));
#12770=DIRECTION('ref_axis',(-0.866025403784439,0.,0.5));
#12771=DIRECTION('',(0.866025403784438,0.,-0.5));
#12772=DIRECTION('',(0.,-1.,0.));
#12773=DIRECTION('center_axis',(0.5,0.,-0.866025403784439));
#12774=DIRECTION('ref_axis',(-0.866025403784439,0.,-0.5));
#12775=DIRECTION('',(0.866025403784439,0.,0.5));
#12776=DIRECTION('',(0.,-1.,0.));
#12777=DIRECTION('center_axis',(1.,0.,0.));
#12778=DIRECTION('ref_axis',(0.,0.,-1.));
#12779=DIRECTION('',(0.,0.,1.));
#12780=DIRECTION('',(0.,-1.,0.));
#12781=DIRECTION('center_axis',(0.5,0.,0.866025403784439));
#12782=DIRECTION('ref_axis',(0.866025403784439,0.,-0.5));
#12783=DIRECTION('',(-0.866025403784438,0.,0.5));
#12784=DIRECTION('',(0.,-1.,0.));
#12785=DIRECTION('center_axis',(-0.5,0.,0.866025403784439));
#12786=DIRECTION('ref_axis',(0.866025403784439,0.,0.5));
#12787=DIRECTION('',(-0.866025403784439,0.,-0.5));
#12788=DIRECTION('center_axis',(0.,1.,0.));
#12789=DIRECTION('ref_axis',(0.,0.,1.));
#12790=DIRECTION('axis',(0.,0.,1.));
#12791=DIRECTION('refdir',(1.,0.,0.));
#12792=DIRECTION('center_axis',(-1.,-1.09403464434161E-29,5.38490012450672E-30));
#12793=DIRECTION('ref_axis',(5.38490012450672E-30,4.73316543132608E-30,
1.));
#12794=DIRECTION('center_axis',(1.,1.09403464434161E-29,5.39106310032879E-30));
#12795=DIRECTION('ref_axis',(5.39106310032879E-30,-6.12323399573724E-17,
-1.));
#12796=DIRECTION('',(-5.38490012450672E-30,1.21234028674329E-16,-1.));
#12797=DIRECTION('center_axis',(-1.,-1.09403464434161E-29,5.38490012450672E-30));
#12798=DIRECTION('ref_axis',(5.38490012450672E-30,4.73316543132608E-30,
1.));
#12799=DIRECTION('',(5.38490012450672E-30,4.73316543132608E-30,1.));
#12800=DIRECTION('center_axis',(-1.,-1.09403464434161E-29,-5.39106310032879E-30));
#12801=DIRECTION('ref_axis',(5.39106310032879E-30,1.17892770941212E-58,
-1.));
#12802=DIRECTION('center_axis',(1.09403464434161E-29,1.,1.21234028674329E-16));
#12803=DIRECTION('ref_axis',(5.38490012450672E-30,-1.21234028674329E-16,
1.));
#12804=DIRECTION('center_axis',(-1.09403464434161E-29,-1.,4.73316543132608E-30));
#12805=DIRECTION('ref_axis',(-5.38490012450672E-30,-4.73316543132608E-30,
-1.));
#12806=DIRECTION('axis',(0.,0.,1.));
#12807=DIRECTION('refdir',(1.,0.,0.));
#12808=DIRECTION('center_axis',(0.,-1.,0.));
#12809=DIRECTION('ref_axis',(0.,0.,-1.));
#12810=DIRECTION('center_axis',(0.,1.,0.));
#12811=DIRECTION('ref_axis',(0.,0.,1.));
#12812=DIRECTION('center_axis',(0.,1.,0.));
#12813=DIRECTION('ref_axis',(0.,0.,1.));
#12814=DIRECTION('',(0.,1.,0.));
#12815=DIRECTION('center_axis',(0.,1.,0.));
#12816=DIRECTION('ref_axis',(0.,0.,1.));
#12817=DIRECTION('center_axis',(0.,1.,0.));
#12818=DIRECTION('ref_axis',(0.,0.,1.));
#12819=DIRECTION('center_axis',(0.,1.,0.));
#12820=DIRECTION('ref_axis',(0.,0.,1.));
#12821=DIRECTION('center_axis',(0.,1.,0.));
#12822=DIRECTION('ref_axis',(0.,0.,1.));
#12823=DIRECTION('center_axis',(0.,-1.,0.));
#12824=DIRECTION('ref_axis',(0.,0.,1.));
#12825=DIRECTION('center_axis',(0.,-1.,0.));
#12826=DIRECTION('ref_axis',(0.,0.,-1.));
#12827=DIRECTION('center_axis',(0.,-1.,0.));
#12828=DIRECTION('ref_axis',(0.,0.,-1.));
#12829=DIRECTION('',(0.,1.,0.));
#12830=DIRECTION('center_axis',(0.,1.,0.));
#12831=DIRECTION('ref_axis',(0.,0.,1.));
#12832=DIRECTION('center_axis',(0.,1.,0.));
#12833=DIRECTION('ref_axis',(0.,0.,1.));
#12834=DIRECTION('',(6.10818125343946E-17,0.,1.));
#12835=DIRECTION('',(-1.,0.,1.12644381556936E-16));
#12836=DIRECTION('',(0.,0.,-1.));
#12837=DIRECTION('',(1.,0.,-1.12644381556936E-16));
#12838=DIRECTION('center_axis',(-1.,0.,6.10818125343946E-17));
#12839=DIRECTION('ref_axis',(6.10818125343946E-17,0.,1.));
#12840=DIRECTION('',(1.58091363932832E-17,0.965925826289068,0.258819045102521));
#12841=DIRECTION('',(6.10818125343946E-17,0.,1.));
#12842=DIRECTION('',(-1.58091363932832E-17,0.965925826289068,-0.258819045102521));
#12843=DIRECTION('center_axis',(1.08806117332204E-16,0.258819045102521,
0.965925826289068));
#12844=DIRECTION('ref_axis',(-2.91545112707301E-17,0.965925826289068,-0.258819045102521));
#12845=DIRECTION('',(-1.,0.,1.12644381556936E-16));
#12846=DIRECTION('',(0.,0.965925826289068,-0.258819045102521));
#12847=DIRECTION('center_axis',(1.,0.,0.));
#12848=DIRECTION('ref_axis',(0.,0.,-1.));
#12849=DIRECTION('',(0.,0.,-1.));
#12850=DIRECTION('',(0.,0.965925826289068,0.258819045102521));
#12851=DIRECTION('center_axis',(-1.08806117332204E-16,0.258819045102521,
-0.965925826289068));
#12852=DIRECTION('ref_axis',(2.91545112707301E-17,0.965925826289068,0.258819045102521));
#12853=DIRECTION('',(1.,0.,-1.12644381556936E-16));
#12854=DIRECTION('center_axis',(0.,1.,0.));
#12855=DIRECTION('ref_axis',(0.,0.,1.));
#12856=DIRECTION('center_axis',(0.,1.,0.));
#12857=DIRECTION('ref_axis',(0.,0.,1.));
#12858=DIRECTION('center_axis',(-1.,0.,1.22464679914735E-16));
#12859=DIRECTION('ref_axis',(-1.22464679914735E-16,0.,-1.));
#12860=DIRECTION('center_axis',(-6.12323399573677E-17,0.,-1.));
#12861=DIRECTION('ref_axis',(-1.,0.,0.));
#12862=DIRECTION('axis',(0.,0.,1.));
#12863=DIRECTION('refdir',(1.,0.,0.));
#12864=DIRECTION('center_axis',(0.,-1.,0.));
#12865=DIRECTION('ref_axis',(0.,0.,-1.));
#12866=DIRECTION('',(0.,0.,-1.));
#12867=DIRECTION('',(-1.,0.,0.));
#12868=DIRECTION('',(0.,0.,1.));
#12869=DIRECTION('',(1.,0.,0.));
#12870=DIRECTION('',(0.,0.,-1.));
#12871=DIRECTION('',(1.,0.,0.));
#12872=DIRECTION('',(0.,0.,1.));
#12873=DIRECTION('',(1.,0.,0.));
#12874=DIRECTION('',(0.,0.,-1.));
#12875=DIRECTION('',(1.,0.,0.));
#12876=DIRECTION('',(0.,0.,1.));
#12877=DIRECTION('',(-1.,0.,0.));
#12878=DIRECTION('',(0.,0.,-1.));
#12879=DIRECTION('',(-1.,0.,0.));
#12880=DIRECTION('',(0.,0.,1.));
#12881=DIRECTION('',(-1.,0.,0.));
#12882=DIRECTION('center_axis',(-1.,0.,0.));
#12883=DIRECTION('ref_axis',(0.,0.,1.));
#12884=DIRECTION('',(0.,0.,-1.));
#12885=DIRECTION('',(0.,-1.,0.));
#12886=DIRECTION('',(0.,-1.,0.));
#12887=DIRECTION('center_axis',(0.,0.,1.));
#12888=DIRECTION('ref_axis',(1.,0.,0.));
#12889=DIRECTION('',(-1.,0.,0.));
#12890=DIRECTION('',(0.,-1.,0.));
#12891=DIRECTION('center_axis',(1.,0.,0.));
#12892=DIRECTION('ref_axis',(0.,0.,-1.));
#12893=DIRECTION('',(0.,0.,1.));
#12894=DIRECTION('',(0.,-1.,0.));
#12895=DIRECTION('center_axis',(0.,0.,-1.));
#12896=DIRECTION('ref_axis',(-1.,0.,0.));
#12897=DIRECTION('',(1.,0.,0.));
#12898=DIRECTION('center_axis',(0.,-1.,0.));
#12899=DIRECTION('ref_axis',(0.,0.,-1.));
#12900=DIRECTION('',(0.,0.,-1.));
#12901=DIRECTION('',(-1.,0.,0.));
#12902=DIRECTION('',(0.,0.,1.));
#12903=DIRECTION('',(-1.,0.,0.));
#12904=DIRECTION('',(0.,0.,-1.));
#12905=DIRECTION('',(-1.,0.,0.));
#12906=DIRECTION('',(0.,0.,1.));
#12907=DIRECTION('',(1.,0.,0.));
#12908=DIRECTION('',(0.,0.,-1.));
#12909=DIRECTION('',(1.,0.,0.));
#12910=DIRECTION('',(0.,0.,1.));
#12911=DIRECTION('',(1.,0.,0.));
#12912=DIRECTION('center_axis',(1.,0.,0.));
#12913=DIRECTION('ref_axis',(0.,0.,-1.));
#12914=DIRECTION('',(0.,1.,0.));
#12915=DIRECTION('',(0.,0.,-1.));
#12916=DIRECTION('',(0.,1.,0.));
#12917=DIRECTION('center_axis',(0.,0.,1.));
#12918=DIRECTION('ref_axis',(1.,0.,0.));
#12919=DIRECTION('',(1.,0.,0.));
#12920=DIRECTION('',(0.,1.,0.));
#12921=DIRECTION('center_axis',(-1.,0.,0.));
#12922=DIRECTION('ref_axis',(0.,0.,1.));
#12923=DIRECTION('',(0.,0.,1.));
#12924=DIRECTION('',(0.,1.,0.));
#12925=DIRECTION('center_axis',(0.,0.,1.));
#12926=DIRECTION('ref_axis',(1.,0.,0.));
#12927=DIRECTION('',(1.,0.,0.));
#12928=DIRECTION('',(0.,1.,0.));
#12929=DIRECTION('center_axis',(1.,0.,0.));
#12930=DIRECTION('ref_axis',(0.,0.,-1.));
#12931=DIRECTION('',(0.,0.,-1.));
#12932=DIRECTION('',(0.,1.,0.));
#12933=DIRECTION('center_axis',(0.,0.,1.));
#12934=DIRECTION('ref_axis',(1.,0.,0.));
#12935=DIRECTION('',(1.,0.,0.));
#12936=DIRECTION('',(0.,1.,0.));
#12937=DIRECTION('center_axis',(-1.,0.,0.));
#12938=DIRECTION('ref_axis',(0.,0.,1.));
#12939=DIRECTION('',(0.,0.,1.));
#12940=DIRECTION('',(0.,1.,0.));
#12941=DIRECTION('center_axis',(0.,0.,-1.));
#12942=DIRECTION('ref_axis',(-1.,0.,0.));
#12943=DIRECTION('',(-1.,0.,0.));
#12944=DIRECTION('',(0.,1.,0.));
#12945=DIRECTION('center_axis',(1.,0.,0.));
#12946=DIRECTION('ref_axis',(0.,0.,-1.));
#12947=DIRECTION('',(0.,0.,-1.));
#12948=DIRECTION('',(0.,1.,0.));
#12949=DIRECTION('center_axis',(0.,0.,-1.));
#12950=DIRECTION('ref_axis',(-1.,0.,0.));
#12951=DIRECTION('',(-1.,0.,0.));
#12952=DIRECTION('',(0.,1.,0.));
#12953=DIRECTION('center_axis',(-1.,0.,0.));
#12954=DIRECTION('ref_axis',(0.,0.,1.));
#12955=DIRECTION('',(0.,0.,1.));
#12956=DIRECTION('',(0.,1.,0.));
#12957=DIRECTION('center_axis',(0.,0.,-1.));
#12958=DIRECTION('ref_axis',(-1.,0.,0.));
#12959=DIRECTION('',(-1.,0.,0.));
#12960=DIRECTION('center_axis',(0.,-1.,0.));
#12961=DIRECTION('ref_axis',(0.,0.,-1.));
#12962=DIRECTION('center_axis',(-1.,0.,0.));
#12963=DIRECTION('ref_axis',(0.,0.,1.));
#12964=DIRECTION('',(0.,-1.,0.));
#12965=DIRECTION('',(0.,0.,-1.));
#12966=DIRECTION('',(0.,-1.,0.));
#12967=DIRECTION('center_axis',(0.,0.,1.));
#12968=DIRECTION('ref_axis',(1.,0.,0.));
#12969=DIRECTION('',(-1.,0.,0.));
#12970=DIRECTION('',(0.,-1.,0.));
#12971=DIRECTION('center_axis',(1.,0.,0.));
#12972=DIRECTION('ref_axis',(0.,0.,-1.));
#12973=DIRECTION('',(0.,0.,1.));
#12974=DIRECTION('',(0.,-1.,0.));
#12975=DIRECTION('center_axis',(0.,0.,1.));
#12976=DIRECTION('ref_axis',(1.,0.,0.));
#12977=DIRECTION('',(-1.,0.,0.));
#12978=DIRECTION('',(0.,-1.,0.));
#12979=DIRECTION('center_axis',(-1.,0.,0.));
#12980=DIRECTION('ref_axis',(0.,0.,1.));
#12981=DIRECTION('',(0.,0.,-1.));
#12982=DIRECTION('',(0.,-1.,0.));
#12983=DIRECTION('center_axis',(0.,0.,1.));
#12984=DIRECTION('ref_axis',(1.,0.,0.));
#12985=DIRECTION('',(-1.,0.,0.));
#12986=DIRECTION('',(0.,-1.,0.));
#12987=DIRECTION('center_axis',(1.,0.,0.));
#12988=DIRECTION('ref_axis',(0.,0.,-1.));
#12989=DIRECTION('',(0.,0.,1.));
#12990=DIRECTION('',(0.,-1.,0.));
#12991=DIRECTION('center_axis',(0.,0.,-1.));
#12992=DIRECTION('ref_axis',(-1.,0.,0.));
#12993=DIRECTION('',(1.,0.,0.));
#12994=DIRECTION('',(0.,-1.,0.));
#12995=DIRECTION('center_axis',(-1.,0.,0.));
#12996=DIRECTION('ref_axis',(0.,0.,1.));
#12997=DIRECTION('',(0.,0.,-1.));
#12998=DIRECTION('',(0.,-1.,0.));
#12999=DIRECTION('center_axis',(0.,0.,-1.));
#13000=DIRECTION('ref_axis',(-1.,0.,0.));
#13001=DIRECTION('',(1.,0.,0.));
#13002=DIRECTION('',(0.,-1.,0.));
#13003=DIRECTION('center_axis',(1.,0.,0.));
#13004=DIRECTION('ref_axis',(0.,0.,-1.));
#13005=DIRECTION('',(0.,0.,1.));
#13006=DIRECTION('',(0.,-1.,0.));
#13007=DIRECTION('center_axis',(0.,0.,-1.));
#13008=DIRECTION('ref_axis',(-1.,0.,0.));
#13009=DIRECTION('',(1.,0.,0.));
#13010=DIRECTION('center_axis',(0.,1.,0.));
#13011=DIRECTION('ref_axis',(0.,0.,-1.));
#13012=DIRECTION('axis',(0.,0.,1.));
#13013=DIRECTION('refdir',(1.,0.,0.));
#13014=DIRECTION('center_axis',(0.,0.,1.));
#13015=DIRECTION('ref_axis',(1.,0.,0.));
#13016=DIRECTION('center_axis',(0.,1.,0.));
#13017=DIRECTION('ref_axis',(0.,0.,1.));
#13018=DIRECTION('center_axis',(0.,0.,-1.));
#13019=DIRECTION('ref_axis',(1.,0.,0.));
#13020=DIRECTION('center_axis',(-0.173648177666917,0.98480775301221,0.));
#13021=DIRECTION('ref_axis',(0.,0.,1.));
#13022=DIRECTION('center_axis',(-0.173648177666917,0.98480775301221,0.));
#13023=DIRECTION('ref_axis',(0.,0.,1.));
#13024=DIRECTION('center_axis',(0.,1.,0.));
#13025=DIRECTION('ref_axis',(0.,0.,1.));
#13026=DIRECTION('axis',(0.,0.,1.));
#13027=DIRECTION('refdir',(1.,0.,0.));
#13028=DIRECTION('center_axis',(7.99859929422742E-44,-1.,0.));
#13029=DIRECTION('ref_axis',(-1.23541874016716E-29,-9.88161946317638E-73,
-1.));
#13030=DIRECTION('center_axis',(-7.99859929422742E-44,1.,0.));
#13031=DIRECTION('ref_axis',(1.23541874016716E-29,9.88161946317638E-73,
1.));
#13032=DIRECTION('',(-7.99859929422742E-44,1.,0.));
#13033=DIRECTION('center_axis',(-7.99859929422742E-44,1.,0.));
#13034=DIRECTION('ref_axis',(1.23541874016716E-29,9.88161946317638E-73,
1.));
#13035=DIRECTION('center_axis',(-7.99859929422742E-44,1.,9.88161946317638E-73));
#13036=DIRECTION('ref_axis',(1.23541874016716E-29,6.83612350571318E-90,
1.));
#13037=DIRECTION('center_axis',(-7.99859929422742E-44,1.,9.88161946317638E-73));
#13038=DIRECTION('ref_axis',(1.23541874016716E-29,6.83612350571318E-90,
1.));
#13039=DIRECTION('axis',(0.,0.,1.));
#13040=DIRECTION('refdir',(1.,0.,0.));
#13041=DIRECTION('center_axis',(0.,1.,0.));
#13042=DIRECTION('ref_axis',(0.,0.,1.));
#13043=DIRECTION('center_axis',(0.,1.,0.));
#13044=DIRECTION('ref_axis',(0.,0.,1.));
#13045=DIRECTION('center_axis',(0.,1.,0.));
#13046=DIRECTION('ref_axis',(0.,0.,1.));
#13047=DIRECTION('center_axis',(0.,1.,0.));
#13048=DIRECTION('ref_axis',(0.,0.,1.));
#13049=DIRECTION('center_axis',(0.,1.,0.));
#13050=DIRECTION('ref_axis',(0.,0.,1.));
#13051=DIRECTION('center_axis',(0.,1.,0.));
#13052=DIRECTION('ref_axis',(0.,0.,1.));
#13053=DIRECTION('center_axis',(0.,-1.,0.));
#13054=DIRECTION('ref_axis',(0.,0.,-1.));
#13055=DIRECTION('',(0.,1.,0.));
#13056=DIRECTION('center_axis',(0.,-1.,0.));
#13057=DIRECTION('ref_axis',(0.,0.,-1.));
#13058=DIRECTION('',(0.,-1.,0.));
#13059=DIRECTION('',(0.,-1.,-3.49148133884313E-15));
#13060=DIRECTION('',(1.,0.,0.));
#13061=DIRECTION('',(-1.03090206175598E-30,1.,3.49148133884314E-15));
#13062=DIRECTION('',(-1.,-8.98665767093703E-31,-3.78739800757717E-17));
#13063=DIRECTION('',(0.950192882786585,0.311662454430621,2.94170160513277E-17));
#13064=DIRECTION('',(-0.311662454430621,0.950192882786585,2.4315639097731E-16));
#13065=DIRECTION('',(-5.55111512312518E-17,-1.,-3.49148133884313E-15));
#13066=DIRECTION('',(1.,-5.55111512312518E-17,-3.94430452610492E-31));
#13067=DIRECTION('',(-1.38777878078154E-17,1.,3.49148133884313E-15));
#13068=DIRECTION('',(-1.,-1.38777878078154E-17,-5.91645678915762E-31));
#13069=DIRECTION('',(-1.,0.,0.));
#13070=DIRECTION('',(0.,-1.,-3.49148133884313E-15));
#13071=DIRECTION('',(0.,-1.,-3.49148133884313E-15));
#13072=DIRECTION('',(1.,0.,0.));
#13073=DIRECTION('',(0.,0.,1.));
#13074=DIRECTION('',(1.,0.,0.));
#13075=DIRECTION('',(-0.588767146052722,0.808302695609098,2.89614564627034E-15));
#13076=DIRECTION('',(0.808302695609098,0.588767146052722,2.12004397610024E-15));
#13077=DIRECTION('',(5.87718104738967E-30,-1.,-3.49148133884313E-15));
#13078=DIRECTION('',(1.,5.87718104738967E-30,7.18906912825122E-45));
#13079=DIRECTION('',(-5.55111512312518E-17,-1.,-3.49148133884313E-15));
#13080=DIRECTION('',(1.,-5.55111512312518E-17,-3.94430452610492E-31));
#13081=DIRECTION('',(0.171796701776671,-0.98513242422461,-3.43957147546953E-15));
#13082=DIRECTION('',(0.98513242422461,0.171796701776671,5.99824978328046E-16));
#13083=DIRECTION('',(-0.425325523710207,-0.905040440466965,-3.15993180878879E-15));
#13084=DIRECTION('',(0.905040440466965,-0.425325523710207,-1.48501612896788E-15));
#13085=DIRECTION('',(0.674646575466201,0.738140906745946,2.69087531904506E-15));
#13086=DIRECTION('',(0.738140906745946,-0.674646575466201,-2.4409704752618E-15));
#13087=DIRECTION('axis',(0.,0.,1.));
#13088=DIRECTION('refdir',(1.,0.,0.));
#13089=DIRECTION('center_axis',(0.,-1.,0.));
#13090=DIRECTION('ref_axis',(0.,0.,-1.));
#13091=DIRECTION('center_axis',(0.,-1.,0.));
#13092=DIRECTION('ref_axis',(0.,0.,-1.));
#13093=DIRECTION('',(0.,1.,0.));
#13094=DIRECTION('center_axis',(0.,-1.,0.));
#13095=DIRECTION('ref_axis',(0.,0.,-1.));
#13096=DIRECTION('center_axis',(0.,1.,0.));
#13097=DIRECTION('ref_axis',(0.,0.,1.));
#13098=DIRECTION('center_axis',(0.,-1.,0.));
#13099=DIRECTION('ref_axis',(0.,0.,-1.));
#13100=DIRECTION('center_axis',(0.,-1.,0.));
#13101=DIRECTION('ref_axis',(0.,0.,-1.));
#13102=DIRECTION('',(0.,1.,0.));
#13103=DIRECTION('center_axis',(0.,-1.,0.));
#13104=DIRECTION('ref_axis',(0.,0.,-1.));
#13105=DIRECTION('center_axis',(0.,-1.,0.));
#13106=DIRECTION('ref_axis',(0.,0.,-1.));
#13107=DIRECTION('center_axis',(0.,1.,0.));
#13108=DIRECTION('ref_axis',(0.,0.,1.));
#13109=DIRECTION('center_axis',(0.,-1.,0.));
#13110=DIRECTION('ref_axis',(0.,0.,-1.));
#13111=DIRECTION('center_axis',(0.,-1.,0.));
#13112=DIRECTION('ref_axis',(0.,0.,-1.));
#13113=DIRECTION('center_axis',(0.,-1.,0.));
#13114=DIRECTION('ref_axis',(0.,0.,-1.));
#13115=DIRECTION('',(0.,1.,0.));
#13116=DIRECTION('center_axis',(0.,-1.,0.));
#13117=DIRECTION('ref_axis',(0.,0.,-1.));
#13118=DIRECTION('center_axis',(0.,-1.,0.));
#13119=DIRECTION('ref_axis',(0.,0.,-1.));
#13120=DIRECTION('center_axis',(0.,1.,0.));
#13121=DIRECTION('ref_axis',(0.,0.,1.));
#13122=DIRECTION('center_axis',(0.,-1.,0.));
#13123=DIRECTION('ref_axis',(0.,0.,-1.));
#13124=DIRECTION('center_axis',(0.,-1.,0.));
#13125=DIRECTION('ref_axis',(0.,0.,-1.));
#13126=DIRECTION('',(0.,1.,0.));
#13127=DIRECTION('axis',(0.,0.,1.));
#13128=DIRECTION('refdir',(1.,0.,0.));
#13129=DIRECTION('axis',(0.,0.,1.));
#13130=DIRECTION('refdir',(1.,0.,0.));
#13131=DIRECTION('center_axis',(0.,0.,1.));
#13132=DIRECTION('ref_axis',(1.,0.,0.));
#13133=DIRECTION('center_axis',(0.,0.,1.));
#13134=DIRECTION('ref_axis',(1.,0.,0.));
#13135=DIRECTION('',(0.,0.,1.));
#13136=DIRECTION('center_axis',(0.,0.,-1.));
#13137=DIRECTION('ref_axis',(-1.,0.,0.));
#13138=DIRECTION('',(0.,0.,-1.));
#13139=DIRECTION('center_axis',(0.,0.,1.));
#13140=DIRECTION('ref_axis',(1.,0.,0.));
#13141=DIRECTION('',(0.,0.,-1.));
#13142=DIRECTION('center_axis',(0.,0.,1.));
#13143=DIRECTION('ref_axis',(1.,0.,0.));
#13144=DIRECTION('',(0.,0.,1.));
#13145=DIRECTION('center_axis',(0.,0.,-1.));
#13146=DIRECTION('ref_axis',(-1.,0.,0.));
#13147=DIRECTION('center_axis',(0.,0.,1.));
#13148=DIRECTION('ref_axis',(1.,0.,0.));
#13149=DIRECTION('',(0.,0.,-1.));
#13150=DIRECTION('center_axis',(0.,0.,1.));
#13151=DIRECTION('ref_axis',(1.,0.,0.));
#13152=DIRECTION('',(0.,0.,1.));
#13153=DIRECTION('center_axis',(0.,0.,-1.));
#13154=DIRECTION('ref_axis',(-1.,0.,0.));
#13155=DIRECTION('center_axis',(0.,0.,1.));
#13156=DIRECTION('ref_axis',(1.,0.,0.));
#13157=DIRECTION('',(0.,0.,-1.));
#13158=DIRECTION('center_axis',(0.,0.,1.));
#13159=DIRECTION('ref_axis',(1.,0.,0.));
#13160=DIRECTION('',(0.,0.,1.));
#13161=DIRECTION('center_axis',(0.,0.,-1.));
#13162=DIRECTION('ref_axis',(-1.,0.,0.));
#13163=DIRECTION('center_axis',(0.,0.,-1.));
#13164=DIRECTION('ref_axis',(-1.,0.,0.));
#13165=DIRECTION('center_axis',(0.,0.,1.));
#13166=DIRECTION('ref_axis',(1.,0.,0.));
#13167=DIRECTION('center_axis',(0.,0.,1.));
#13168=DIRECTION('ref_axis',(1.,0.,0.));
#13169=DIRECTION('',(0.,0.,1.));
#13170=DIRECTION('center_axis',(0.,0.,-1.));
#13171=DIRECTION('ref_axis',(-1.,0.,0.));
#13172=DIRECTION('',(0.,0.,-1.));
#13173=DIRECTION('center_axis',(0.,0.,1.));
#13174=DIRECTION('ref_axis',(1.,0.,0.));
#13175=DIRECTION('',(0.,0.,-1.));
#13176=DIRECTION('center_axis',(0.,0.,1.));
#13177=DIRECTION('ref_axis',(1.,0.,0.));
#13178=DIRECTION('',(0.,0.,1.));
#13179=DIRECTION('center_axis',(0.,0.,-1.));
#13180=DIRECTION('ref_axis',(-1.,0.,0.));
#13181=DIRECTION('center_axis',(0.,0.,1.));
#13182=DIRECTION('ref_axis',(1.,0.,0.));
#13183=DIRECTION('',(0.,0.,-1.));
#13184=DIRECTION('center_axis',(0.,0.,1.));
#13185=DIRECTION('ref_axis',(1.,0.,0.));
#13186=DIRECTION('',(0.,0.,1.));
#13187=DIRECTION('center_axis',(0.,0.,-1.));
#13188=DIRECTION('ref_axis',(-1.,0.,0.));
#13189=DIRECTION('center_axis',(0.,0.,1.));
#13190=DIRECTION('ref_axis',(1.,0.,0.));
#13191=DIRECTION('',(0.,0.,-1.));
#13192=DIRECTION('center_axis',(0.,0.,1.));
#13193=DIRECTION('ref_axis',(1.,0.,0.));
#13194=DIRECTION('',(0.,0.,1.));
#13195=DIRECTION('center_axis',(0.,0.,-1.));
#13196=DIRECTION('ref_axis',(-1.,0.,0.));
#13197=DIRECTION('center_axis',(0.,0.,1.));
#13198=DIRECTION('ref_axis',(-0.999999999999999,4.09856065867257E-8,0.));
#13199=DIRECTION('',(0.,0.,-1.));
#13200=DIRECTION('center_axis',(0.,0.,1.));
#13201=DIRECTION('ref_axis',(1.,0.,0.));
#13202=DIRECTION('',(0.,0.,1.));
#13203=DIRECTION('center_axis',(0.,0.,-1.));
#13204=DIRECTION('ref_axis',(-1.,0.,0.));
#13205=DIRECTION('center_axis',(0.,0.,1.));
#13206=DIRECTION('ref_axis',(1.,0.,0.));
#13207=DIRECTION('center_axis',(0.,0.,1.));
#13208=DIRECTION('ref_axis',(1.,0.,0.));
#13209=DIRECTION('center_axis',(0.,0.,1.));
#13210=DIRECTION('ref_axis',(1.,0.,0.));
#13211=DIRECTION('center_axis',(0.,0.,1.));
#13212=DIRECTION('ref_axis',(1.,0.,0.));
#13213=DIRECTION('center_axis',(0.,0.,1.));
#13214=DIRECTION('ref_axis',(1.,0.,0.));
#13215=DIRECTION('center_axis',(0.,0.,1.));
#13216=DIRECTION('ref_axis',(1.,0.,0.));
#13217=DIRECTION('center_axis',(0.,0.,1.));
#13218=DIRECTION('ref_axis',(1.,0.,0.));
#13219=DIRECTION('center_axis',(0.,0.,1.));
#13220=DIRECTION('ref_axis',(1.,0.,0.));
#13221=DIRECTION('center_axis',(0.,0.,1.));
#13222=DIRECTION('ref_axis',(1.,0.,0.));
#13223=DIRECTION('center_axis',(0.,0.,1.));
#13224=DIRECTION('ref_axis',(1.,0.,0.));
#13225=DIRECTION('center_axis',(0.,0.,1.));
#13226=DIRECTION('ref_axis',(1.,0.,0.));
#13227=DIRECTION('center_axis',(0.,0.,1.));
#13228=DIRECTION('ref_axis',(1.,0.,0.));
#13229=DIRECTION('center_axis',(0.,0.,-1.));
#13230=DIRECTION('ref_axis',(-1.,0.,0.));
#13231=DIRECTION('center_axis',(0.,0.,-1.));
#13232=DIRECTION('ref_axis',(-1.,0.,0.));
#13233=DIRECTION('center_axis',(0.,0.,1.));
#13234=DIRECTION('ref_axis',(1.,0.,0.));
#13235=DIRECTION('',(0.,0.,-1.));
#13236=DIRECTION('center_axis',(0.,0.,-1.));
#13237=DIRECTION('ref_axis',(-1.,0.,0.));
#13238=DIRECTION('center_axis',(0.,0.,-1.));
#13239=DIRECTION('ref_axis',(-1.,0.,0.));
#13240=DIRECTION('center_axis',(0.,0.,-1.));
#13241=DIRECTION('ref_axis',(-1.,0.,0.));
#13242=DIRECTION('',(0.,0.,-1.));
#13243=DIRECTION('center_axis',(0.,0.,1.));
#13244=DIRECTION('ref_axis',(1.,0.,0.));
#13245=DIRECTION('center_axis',(0.,0.,1.));
#13246=DIRECTION('ref_axis',(1.,0.,0.));
#13247=DIRECTION('',(0.,0.,-1.));
#13248=DIRECTION('',(0.,0.,1.));
#13249=DIRECTION('center_axis',(0.,0.,-1.));
#13250=DIRECTION('ref_axis',(-1.,0.,0.));
#13251=DIRECTION('center_axis',(0.,0.,-1.));
#13252=DIRECTION('ref_axis',(-1.,0.,0.));
#13253=DIRECTION('center_axis',(0.,0.,1.));
#13254=DIRECTION('ref_axis',(1.,0.,0.));
#13255=DIRECTION('center_axis',(0.,0.,1.));
#13256=DIRECTION('ref_axis',(1.,0.,0.));
#13257=DIRECTION('center_axis',(0.,0.,-1.));
#13258=DIRECTION('ref_axis',(-1.,0.,0.));
#13259=DIRECTION('center_axis',(0.,0.,1.));
#13260=DIRECTION('ref_axis',(1.,0.,0.));
#13261=DIRECTION('center_axis',(0.,0.,1.));
#13262=DIRECTION('ref_axis',(1.,0.,0.));
#13263=DIRECTION('',(-0.028249590671202,3.45957707927105E-18,0.999600900673318));
#13264=DIRECTION('center_axis',(0.,0.,1.));
#13265=DIRECTION('ref_axis',(1.,0.,0.));
#13266=DIRECTION('',(0.,0.,-1.));
#13267=DIRECTION('center_axis',(0.,0.,1.));
#13268=DIRECTION('ref_axis',(1.,0.,0.));
#13269=DIRECTION('center_axis',(0.,0.,-1.));
#13270=DIRECTION('ref_axis',(-1.,0.,0.));
#13271=DIRECTION('center_axis',(0.,0.,1.));
#13272=DIRECTION('ref_axis',(1.,0.,0.));
#13273=DIRECTION('center_axis',(0.,0.,1.));
#13274=DIRECTION('ref_axis',(1.,0.,0.));
#13275=DIRECTION('',(0.,0.,-1.));
#13276=DIRECTION('center_axis',(0.,0.,1.));
#13277=DIRECTION('ref_axis',(1.,0.,0.));
#13278=DIRECTION('center_axis',(0.,0.,1.));
#13279=DIRECTION('ref_axis',(1.,0.,0.));
#13280=DIRECTION('center_axis',(0.,0.,-1.));
#13281=DIRECTION('ref_axis',(-1.,0.,0.));
#13282=DIRECTION('',(-0.707106781186543,8.65956056235487E-17,0.707106781186552));
#13283=DIRECTION('center_axis',(0.,0.,1.));
#13284=DIRECTION('ref_axis',(1.,0.,0.));
#13285=DIRECTION('center_axis',(0.,0.,1.));
#13286=DIRECTION('ref_axis',(1.,0.,0.));
#13287=DIRECTION('center_axis',(0.,0.,1.));
#13288=DIRECTION('ref_axis',(1.,0.,0.));
#13289=DIRECTION('',(0.,0.,1.));
#13290=DIRECTION('center_axis',(0.,1.,0.));
#13291=DIRECTION('ref_axis',(0.,0.,1.));
#13292=DIRECTION('',(0.,1.,0.));
#13293=DIRECTION('center_axis',(-0.951056516295155,0.309016994374945,0.));
#13294=DIRECTION('ref_axis',(-0.309016994374945,-0.951056516295155,0.));
#13295=DIRECTION('',(-0.951056516295154,0.309016994374945,0.));
#13296=DIRECTION('center_axis',(0.95105651629515,0.309016994374958,0.));
#13297=DIRECTION('ref_axis',(-0.309016994374958,0.95105651629515,0.));
#13298=DIRECTION('',(0.95105651629515,0.309016994374958,0.));
#13299=DIRECTION('center_axis',(0.58778525229248,-0.809016994374942,0.));
#13300=DIRECTION('ref_axis',(0.809016994374942,0.58778525229248,0.));
#13301=DIRECTION('',(0.58778525229248,-0.809016994374942,0.));
#13302=DIRECTION('center_axis',(-0.587785252292469,-0.809016994374951,0.));
#13303=DIRECTION('ref_axis',(0.809016994374951,-0.587785252292469,0.));
#13304=DIRECTION('',(-0.587785252292469,-0.809016994374951,0.));
#13305=DIRECTION('center_axis',(0.,0.,-1.));
#13306=DIRECTION('ref_axis',(-1.,0.,0.));
#13307=DIRECTION('center_axis',(0.,0.,1.));
#13308=DIRECTION('ref_axis',(-1.,0.,0.));
#13309=DIRECTION('',(0.,0.,-1.));
#13310=DIRECTION('center_axis',(0.,0.,-1.));
#13311=DIRECTION('ref_axis',(-1.,0.,0.));
#13312=DIRECTION('',(0.707106781186551,-8.65956056235497E-17,-0.707106781186544));
#13313=DIRECTION('center_axis',(0.,0.,1.));
#13314=DIRECTION('ref_axis',(1.,0.,0.));
#13315=DIRECTION('center_axis',(0.,0.,1.));
#13316=DIRECTION('ref_axis',(1.,0.,0.));
#13317=DIRECTION('center_axis',(0.,0.,1.));
#13318=DIRECTION('ref_axis',(1.,0.,0.));
#13319=DIRECTION('',(0.,0.,1.));
#13320=DIRECTION('center_axis',(0.,0.,1.));
#13321=DIRECTION('ref_axis',(1.,0.,0.));
#13322=DIRECTION('center_axis',(0.,0.,-1.));
#13323=DIRECTION('ref_axis',(-1.,0.,0.));
#13324=DIRECTION('center_axis',(0.,0.,-1.));
#13325=DIRECTION('ref_axis',(-1.,0.,0.));
#13326=DIRECTION('',(0.,0.,-1.));
#13327=DIRECTION('center_axis',(0.,0.,-1.));
#13328=DIRECTION('ref_axis',(1.,0.,0.));
#13329=DIRECTION('',(0.,0.,1.));
#13330=DIRECTION('center_axis',(0.,0.,-1.));
#13331=DIRECTION('ref_axis',(0.951056370825966,-0.309017442082712,0.));
#13332=DIRECTION('',(0.,0.,-1.));
#13333=DIRECTION('center_axis',(0.,0.,-1.));
#13334=DIRECTION('ref_axis',(1.,0.,0.));
#13335=DIRECTION('',(0.,0.,1.));
#13336=DIRECTION('center_axis',(0.,0.,-1.));
#13337=DIRECTION('ref_axis',(0.951056516295154,0.309016994374948,0.));
#13338=DIRECTION('',(0.,0.,-1.));
#13339=DIRECTION('center_axis',(0.,0.,-1.));
#13340=DIRECTION('ref_axis',(1.,-3.47868984768418E-15,0.));
#13341=DIRECTION('',(0.,0.,1.));
#13342=DIRECTION('center_axis',(0.,0.,-1.));
#13343=DIRECTION('ref_axis',(-1.,0.,0.));
#13344=DIRECTION('',(0.,0.,-1.));
#13345=DIRECTION('center_axis',(0.,0.,-1.));
#13346=DIRECTION('ref_axis',(1.,-7.73042188374262E-16,0.));
#13347=DIRECTION('',(0.,0.,1.));
#13348=DIRECTION('center_axis',(0.,0.,-1.));
#13349=DIRECTION('ref_axis',(-1.,0.,0.));
#13350=DIRECTION('',(0.,0.,-1.));
#13351=DIRECTION('center_axis',(0.,0.,-1.));
#13352=DIRECTION('ref_axis',(1.,0.,0.));
#13353=DIRECTION('',(0.,0.,1.));
#13354=DIRECTION('center_axis',(0.,0.,-1.));
#13355=DIRECTION('ref_axis',(-1.,0.,0.));
#13356=DIRECTION('',(0.,0.,-1.));
#13357=DIRECTION('center_axis',(0.,0.,-1.));
#13358=DIRECTION('ref_axis',(1.,0.,0.));
#13359=DIRECTION('',(0.,0.,1.));
#13360=DIRECTION('center_axis',(0.,0.,-1.));
#13361=DIRECTION('ref_axis',(-1.,0.,0.));
#13362=DIRECTION('',(0.,0.,-1.));
#13363=DIRECTION('center_axis',(0.,0.,-1.));
#13364=DIRECTION('ref_axis',(1.,9.66302735467828E-16,0.));
#13365=DIRECTION('',(0.,0.,1.));
#13366=DIRECTION('center_axis',(0.,0.,-1.));
#13367=DIRECTION('ref_axis',(-1.,0.,0.));
#13368=DIRECTION('',(0.,0.,-1.));
#13369=DIRECTION('center_axis',(0.,0.,-1.));
#13370=DIRECTION('ref_axis',(1.,1.73934492384209E-15,0.));
#13371=DIRECTION('',(0.,0.,1.));
#13372=DIRECTION('center_axis',(0.,0.,-1.));
#13373=DIRECTION('ref_axis',(-1.,0.,0.));
#13374=DIRECTION('',(0.,0.,-1.));
#13375=DIRECTION('center_axis',(0.,0.,-1.));
#13376=DIRECTION('ref_axis',(1.,7.73042188374263E-16,0.));
#13377=DIRECTION('',(0.,0.,1.));
#13378=DIRECTION('center_axis',(0.,0.,-1.));
#13379=DIRECTION('ref_axis',(-1.,0.,0.));
#13380=DIRECTION('',(0.,0.,-1.));
#13381=DIRECTION('center_axis',(0.,0.,-1.));
#13382=DIRECTION('ref_axis',(1.,0.,0.));
#13383=DIRECTION('',(0.,0.,1.));
#13384=DIRECTION('center_axis',(-0.133354245949418,0.449306005611305,-0.883368982027825));
#13385=DIRECTION('ref_axis',(-0.236981598329056,0.85101681114339,0.468625766688881));
#13386=DIRECTION('center_axis',(0.,0.,-1.));
#13387=DIRECTION('ref_axis',(-1.,0.,0.));
#13388=DIRECTION('center_axis',(0.,0.,1.));
#13389=DIRECTION('ref_axis',(1.,0.,0.));
#13390=DIRECTION('center_axis',(0.,0.,1.));
#13391=DIRECTION('ref_axis',(1.,0.,0.));
#13392=DIRECTION('center_axis',(0.156188207235421,0.441878562474938,-0.883373409123043));
#13393=DIRECTION('ref_axis',(0.308715861485718,0.827704076309612,0.468615491557399));
#13394=DIRECTION('center_axis',(0.,0.,-1.));
#13395=DIRECTION('ref_axis',(-1.,0.,0.));
#13396=DIRECTION('center_axis',(0.,0.,1.));
#13397=DIRECTION('ref_axis',(1.,0.,0.));
#13398=DIRECTION('center_axis',(0.,0.,1.));
#13399=DIRECTION('ref_axis',(-0.951056516295154,-0.309016994374948,0.));
#13400=DIRECTION('center_axis',(0.,0.,-1.));
#13401=DIRECTION('ref_axis',(0.995706539546764,-0.0925661228733769,0.));
#13402=DIRECTION('center_axis',(0.,0.,1.));
#13403=DIRECTION('ref_axis',(1.,0.,0.));
#13404=DIRECTION('center_axis',(0.,0.,1.));
#13405=DIRECTION('ref_axis',(-0.951056516295153,0.309016994374948,0.));
#13406=DIRECTION('center_axis',(0.468516296465704,-0.0119958265706286,-0.883373409205274));
#13407=DIRECTION('ref_axis',(0.88259180291303,-0.0378316095121115,0.468615491370537));
#13408=DIRECTION('center_axis',(0.,0.,-1.));
#13409=DIRECTION('ref_axis',(-1.,0.,0.));
#13410=DIRECTION('center_axis',(0.,0.,1.));
#13411=DIRECTION('ref_axis',(1.,0.,0.));
#13412=DIRECTION('center_axis',(0.,0.,1.));
#13413=DIRECTION('ref_axis',(1.,0.,0.));
#13414=DIRECTION('center_axis',(0.,0.,-1.));
#13415=DIRECTION('ref_axis',(-1.,0.,0.));
#13416=DIRECTION('center_axis',(0.,0.,1.));
#13417=DIRECTION('ref_axis',(1.,0.,0.));
#13418=DIRECTION('center_axis',(0.,0.,1.));
#13419=DIRECTION('ref_axis',(1.,0.,0.));
#13420=DIRECTION('center_axis',(0.133354245974411,-0.449306005592514,-0.88336898203361));
#13421=DIRECTION('ref_axis',(-0.23698159806395,0.851016811224501,-0.468625766675648));
#13422=DIRECTION('center_axis',(0.,0.,-1.));
#13423=DIRECTION('ref_axis',(-1.,0.,0.));
#13424=DIRECTION('center_axis',(0.,0.,1.));
#13425=DIRECTION('ref_axis',(1.,0.,0.));
#13426=DIRECTION('center_axis',(0.,0.,1.));
#13427=DIRECTION('ref_axis',(1.,0.,0.));
#13428=DIRECTION('center_axis',(-0.156188207223913,-0.441878562475276,-0.883373409124909));
#13429=DIRECTION('ref_axis',(0.308715861503055,0.827704076305292,-0.468615491553608));
#13430=DIRECTION('center_axis',(0.,0.,-1.));
#13431=DIRECTION('ref_axis',(-1.,0.,0.));
#13432=DIRECTION('center_axis',(0.,0.,1.));
#13433=DIRECTION('ref_axis',(-0.995706539546737,-0.0925661228736592,0.));
#13434=DIRECTION('center_axis',(0.,0.,1.));
#13435=DIRECTION('ref_axis',(1.,0.,0.));
#13436=DIRECTION('center_axis',(0.,0.,-1.));
#13437=DIRECTION('ref_axis',(-1.,0.,0.));
#13438=DIRECTION('center_axis',(0.,0.,1.));
#13439=DIRECTION('ref_axis',(1.,0.,0.));
#13440=DIRECTION('center_axis',(0.,0.,1.));
#13441=DIRECTION('ref_axis',(1.,0.,0.));
#13442=DIRECTION('center_axis',(-0.468516296601123,0.0119958269794971,-0.883373409127899));
#13443=DIRECTION('ref_axis',(0.882591802968309,-0.0378316060417926,-0.468615491546586));
#13444=DIRECTION('center_axis',(0.,0.,-1.));
#13445=DIRECTION('ref_axis',(-1.,0.,0.));
#13446=DIRECTION('center_axis',(0.,0.,1.));
#13447=DIRECTION('ref_axis',(1.,0.,0.));
#13448=DIRECTION('center_axis',(0.,0.,1.));
#13449=DIRECTION('ref_axis',(1.,0.,0.));
#13450=DIRECTION('center_axis',(0.,0.,-1.));
#13451=DIRECTION('ref_axis',(-1.,0.,0.));
#13452=DIRECTION('center_axis',(0.,0.,1.));
#13453=DIRECTION('ref_axis',(1.,0.,0.));
#13454=DIRECTION('center_axis',(0.,0.,1.));
#13455=DIRECTION('ref_axis',(1.,0.,0.));
#13456=DIRECTION('axis',(0.,0.,1.));
#13457=DIRECTION('refdir',(1.,0.,0.));
#13458=DIRECTION('center_axis',(0.,0.,1.));
#13459=DIRECTION('ref_axis',(1.,0.,0.));
#13460=DIRECTION('center_axis',(0.,0.,1.));
#13461=DIRECTION('ref_axis',(1.,0.,0.));
#13462=DIRECTION('center_axis',(0.,0.,-1.));
#13463=DIRECTION('ref_axis',(-1.,0.,0.));
#13464=DIRECTION('center_axis',(0.,0.,-1.));
#13465=DIRECTION('ref_axis',(-1.,0.,0.));
#13466=DIRECTION('center_axis',(0.,0.,1.));
#13467=DIRECTION('ref_axis',(-1.,0.,0.));
#13468=DIRECTION('',(-0.866025403784438,-0.5,0.));
#13469=DIRECTION('',(-0.5,-0.866025403784438,0.));
#13470=DIRECTION('',(-1.,1.1556266144132E-16,0.));
#13471=DIRECTION('',(-0.866025403784438,-0.5,0.));
#13472=DIRECTION('',(-0.866025403784438,0.5,0.));
#13473=DIRECTION('',(-1.,1.1556266144132E-16,0.));
#13474=DIRECTION('',(-0.5,0.866025403784438,0.));
#13475=DIRECTION('',(-0.866025403784438,0.5,0.));
#13476=DIRECTION('',(-1.1556266144132E-16,1.,0.));
#13477=DIRECTION('',(-0.5,0.866025403784438,0.));
#13478=DIRECTION('',(0.5,0.866025403784439,0.));
#13479=DIRECTION('',(-1.1556266144132E-16,1.,0.));
#13480=DIRECTION('',(0.866025403784438,0.5,0.));
#13481=DIRECTION('',(0.5,0.866025403784438,0.));
#13482=DIRECTION('',(1.,1.1556266144132E-16,0.));
#13483=DIRECTION('',(0.866025403784438,0.5,0.));
#13484=DIRECTION('',(0.866025403784438,-0.5,0.));
#13485=DIRECTION('',(1.,1.1556266144132E-16,0.));
#13486=DIRECTION('',(0.5,-0.866025403784438,0.));
#13487=DIRECTION('',(0.866025403784438,-0.5,0.));
#13488=DIRECTION('',(0.,-1.,0.));
#13489=DIRECTION('',(0.5,-0.866025403784438,0.));
#13490=DIRECTION('',(-0.5,-0.866025403784438,0.));
#13491=DIRECTION('',(0.,-1.,0.));
#13492=DIRECTION('center_axis',(0.866025403784439,-0.5,0.));
#13493=DIRECTION('ref_axis',(0.5,0.866025403784439,0.));
#13494=DIRECTION('',(0.5,0.866025403784439,0.));
#13495=DIRECTION('',(0.,0.,1.));
#13496=DIRECTION('',(0.,0.,1.));
#13497=DIRECTION('center_axis',(1.1556266144132E-16,-1.,0.));
#13498=DIRECTION('ref_axis',(1.,1.1556266144132E-16,0.));
#13499=DIRECTION('',(1.,1.1556266144132E-16,0.));
#13500=DIRECTION('',(0.,0.,1.));
#13501=DIRECTION('',(0.,0.,1.));
#13502=DIRECTION('center_axis',(-0.866025403784439,-0.5,0.));
#13503=DIRECTION('ref_axis',(0.5,-0.866025403784439,0.));
#13504=DIRECTION('',(0.5,-0.866025403784438,0.));
#13505=DIRECTION('',(0.,0.,1.));
#13506=DIRECTION('',(0.,0.,1.));
#13507=DIRECTION('center_axis',(-0.866025403784439,0.5,0.));
#13508=DIRECTION('ref_axis',(-0.5,-0.866025403784439,0.));
#13509=DIRECTION('',(0.,0.,-1.));
#13510=DIRECTION('',(-0.5,-0.866025403784438,0.));
#13511=DIRECTION('',(0.,0.,1.));
#13512=DIRECTION('center_axis',(1.1556266144132E-16,1.,0.));
#13513=DIRECTION('ref_axis',(-1.,1.1556266144132E-16,0.));
#13514=DIRECTION('',(-1.,1.1556266144132E-16,0.));
#13515=DIRECTION('',(0.,0.,1.));
#13516=DIRECTION('center_axis',(0.866025403784438,0.5,0.));
#13517=DIRECTION('ref_axis',(-0.5,0.866025403784438,0.));
#13518=DIRECTION('',(-0.5,0.866025403784438,0.));
#13519=DIRECTION('',(0.,0.,1.));
#13520=DIRECTION('',(0.,0.,1.));
#13521=DIRECTION('center_axis',(0.,0.,-1.));
#13522=DIRECTION('ref_axis',(-1.,0.,0.));
#13523=DIRECTION('center_axis',(0.,0.,1.));
#13524=DIRECTION('ref_axis',(1.,0.,0.));
#13525=DIRECTION('center_axis',(0.,0.,1.));
#13526=DIRECTION('ref_axis',(1.,0.,0.));
#13527=DIRECTION('',(0.,0.,-1.));
#13528=DIRECTION('center_axis',(0.,0.,1.));
#13529=DIRECTION('ref_axis',(1.,0.,0.));
#13530=DIRECTION('center_axis',(0.,0.,-1.));
#13531=DIRECTION('ref_axis',(-1.,0.,0.));
#13532=DIRECTION('center_axis',(0.,0.,-1.));
#13533=DIRECTION('ref_axis',(-1.,0.,0.));
#13534=DIRECTION('',(0.,0.,-1.));
#13535=DIRECTION('center_axis',(0.,0.,1.));
#13536=DIRECTION('ref_axis',(1.,0.,0.));
#13537=DIRECTION('center_axis',(0.,0.,1.));
#13538=DIRECTION('ref_axis',(1.,0.,0.));
#13539=DIRECTION('',(0.5,-0.866025403784438,0.));
#13540=DIRECTION('',(0.,-1.,0.));
#13541=DIRECTION('',(0.866025403784438,-0.5,0.));
#13542=DIRECTION('',(1.,1.1556266144132E-16,0.));
#13543=DIRECTION('',(0.866025403784438,-0.5,0.));
#13544=DIRECTION('',(0.866025403784438,0.5,0.));
#13545=DIRECTION('',(0.5,0.866025403784439,0.));
#13546=DIRECTION('',(0.866025403784438,0.5,0.));
#13547=DIRECTION('',(-1.1556266144132E-16,1.,0.));
#13548=DIRECTION('',(-0.5,0.866025403784438,0.));
#13549=DIRECTION('',(-1.1556266144132E-16,1.,0.));
#13550=DIRECTION('',(-0.866025403784438,0.5,0.));
#13551=DIRECTION('',(-1.,1.1556266144132E-16,0.));
#13552=DIRECTION('',(-0.866025403784438,0.5,0.));
#13553=DIRECTION('',(-0.866025403784438,-0.5,0.));
#13554=DIRECTION('',(-0.866025403784438,-0.5,0.));
#13555=DIRECTION('',(0.,-1.,0.));
#13556=DIRECTION('',(-0.5,-0.866025403784438,0.));
#13557=DIRECTION('center_axis',(0.,0.,-1.));
#13558=DIRECTION('ref_axis',(1.,0.,0.));
#13559=DIRECTION('center_axis',(0.866025403784439,-0.5,0.));
#13560=DIRECTION('ref_axis',(0.5,0.866025403784439,0.));
#13561=DIRECTION('',(0.,0.,-1.));
#13562=DIRECTION('center_axis',(1.1556266144132E-16,-1.,0.));
#13563=DIRECTION('ref_axis',(1.,1.1556266144132E-16,0.));
#13564=DIRECTION('',(0.,0.,-1.));
#13565=DIRECTION('center_axis',(-0.866025403784439,-0.5,0.));
#13566=DIRECTION('ref_axis',(0.5,-0.866025403784439,0.));
#13567=DIRECTION('',(0.,0.,-1.));
#13568=DIRECTION('',(0.,0.,1.));
#13569=DIRECTION('center_axis',(-0.866025403784439,0.5,0.));
#13570=DIRECTION('ref_axis',(-0.5,-0.866025403784439,0.));
#13571=DIRECTION('',(0.,0.,1.));
#13572=DIRECTION('center_axis',(1.1556266144132E-16,1.,0.));
#13573=DIRECTION('ref_axis',(-1.,1.1556266144132E-16,0.));
#13574=DIRECTION('',(0.,0.,-1.));
#13575=DIRECTION('center_axis',(0.866025403784438,0.5,0.));
#13576=DIRECTION('ref_axis',(-0.5,0.866025403784438,0.));
#13577=DIRECTION('',(0.,0.,-1.));
#13578=DIRECTION('center_axis',(1.,1.1556266144132E-16,0.));
#13579=DIRECTION('ref_axis',(-1.1556266144132E-16,1.,0.));
#13580=DIRECTION('',(0.,0.,1.));
#13581=DIRECTION('center_axis',(0.5,0.866025403784439,0.));
#13582=DIRECTION('ref_axis',(-0.866025403784439,0.5,0.));
#13583=DIRECTION('center_axis',(0.5,0.866025403784439,0.));
#13584=DIRECTION('ref_axis',(-0.866025403784439,0.5,0.));
#13585=DIRECTION('',(0.,0.,1.));
#13586=DIRECTION('center_axis',(-0.5,0.866025403784439,0.));
#13587=DIRECTION('ref_axis',(-0.866025403784439,-0.5,0.));
#13588=DIRECTION('center_axis',(-1.,0.,0.));
#13589=DIRECTION('ref_axis',(0.,0.,1.));
#13590=DIRECTION('',(0.,0.,1.));
#13591=DIRECTION('center_axis',(-0.5,0.866025403784439,0.));
#13592=DIRECTION('ref_axis',(-0.866025403784439,-0.5,0.));
#13593=DIRECTION('center_axis',(-1.,0.,0.));
#13594=DIRECTION('ref_axis',(0.,0.,1.));
#13595=DIRECTION('',(0.,0.,1.));
#13596=DIRECTION('center_axis',(-0.5,-0.866025403784439,0.));
#13597=DIRECTION('ref_axis',(0.866025403784439,-0.5,0.));
#13598=DIRECTION('center_axis',(-0.5,-0.866025403784439,0.));
#13599=DIRECTION('ref_axis',(0.866025403784439,-0.5,0.));
#13600=DIRECTION('',(0.,0.,1.));
#13601=DIRECTION('center_axis',(0.5,-0.866025403784439,0.));
#13602=DIRECTION('ref_axis',(0.866025403784439,0.5,0.));
#13603=DIRECTION('center_axis',(0.5,-0.866025403784439,0.));
#13604=DIRECTION('ref_axis',(0.866025403784439,0.5,0.));
#13605=DIRECTION('',(0.,0.,1.));
#13606=DIRECTION('center_axis',(1.,1.1556266144132E-16,0.));
#13607=DIRECTION('ref_axis',(-1.1556266144132E-16,1.,0.));
#13608=DIRECTION('center_axis',(0.,0.,1.));
#13609=DIRECTION('ref_axis',(1.,0.,0.));
#13610=DIRECTION('',(-0.866025403784439,-1.06057523872491E-16,0.499999999999999));
#13611=DIRECTION('center_axis',(0.,0.,-1.));
#13612=DIRECTION('ref_axis',(-1.,0.,0.));
#13613=DIRECTION('center_axis',(-1.22464679914735E-16,-1.,0.));
#13614=DIRECTION('ref_axis',(1.,-1.22464679914735E-16,0.));
#13615=DIRECTION('center_axis',(0.,0.,1.));
#13616=DIRECTION('ref_axis',(1.,0.,0.));
#13617=DIRECTION('',(0.707106781186553,8.659560562355E-17,-0.707106781186542));
#13618=DIRECTION('axis',(0.,0.,1.));
#13619=DIRECTION('refdir',(1.,0.,0.));
#13620=DIRECTION('center_axis',(1.,0.,5.58637014214901E-14));
#13621=DIRECTION('ref_axis',(5.58637014214901E-14,0.,-1.));
#13622=DIRECTION('center_axis',(1.,0.,0.));
#13623=DIRECTION('ref_axis',(0.,0.,-1.));
#13624=DIRECTION('center_axis',(1.,0.,0.));
#13625=DIRECTION('ref_axis',(0.,0.,-1.));
#13626=DIRECTION('center_axis',(1.,0.,5.58637014214901E-14));
#13627=DIRECTION('ref_axis',(5.58637014214901E-14,0.,-1.));
#13628=DIRECTION('center_axis',(1.,0.,0.));
#13629=DIRECTION('ref_axis',(0.,0.,-1.));
#13630=DIRECTION('center_axis',(1.,0.,5.58637014214901E-14));
#13631=DIRECTION('ref_axis',(5.58637014214901E-14,0.,-1.));
#13632=DIRECTION('center_axis',(1.,0.,0.));
#13633=DIRECTION('ref_axis',(0.,0.,-1.));
#13634=DIRECTION('center_axis',(1.,0.,5.58637014214901E-14));
#13635=DIRECTION('ref_axis',(5.58637014214901E-14,0.,-1.));
#13636=DIRECTION('center_axis',(1.,0.,5.58637014214901E-14));
#13637=DIRECTION('ref_axis',(5.58637014214901E-14,0.,-1.));
#13638=DIRECTION('center_axis',(1.,0.,0.));
#13639=DIRECTION('ref_axis',(0.,0.,-1.));
#13640=DIRECTION('axis',(0.,0.,1.));
#13641=DIRECTION('refdir',(1.,0.,0.));
#13642=DIRECTION('center_axis',(0.,1.,0.));
#13643=DIRECTION('ref_axis',(0.,0.,1.));
#13644=DIRECTION('center_axis',(0.,-1.,0.));
#13645=DIRECTION('ref_axis',(0.,0.,-1.));
#13646=DIRECTION('center_axis',(0.,-1.,0.));
#13647=DIRECTION('ref_axis',(0.,0.,-1.));
#13648=DIRECTION('center_axis',(0.,-1.,0.));
#13649=DIRECTION('ref_axis',(0.,0.,-1.));
#13650=DIRECTION('',(0.,1.,0.));
#13651=DIRECTION('center_axis',(0.,-1.,0.));
#13652=DIRECTION('ref_axis',(0.,0.,-1.));
#13653=DIRECTION('center_axis',(0.,-1.,0.));
#13654=DIRECTION('ref_axis',(0.,0.,-1.));
#13655=DIRECTION('center_axis',(1.,0.,1.22464679914735E-16));
#13656=DIRECTION('ref_axis',(-1.22464679914735E-16,0.,1.));
#13657=DIRECTION('center_axis',(0.,-1.,0.));
#13658=DIRECTION('ref_axis',(0.,0.,-1.));
#13659=DIRECTION('center_axis',(0.,-1.,0.));
#13660=DIRECTION('ref_axis',(0.,0.,-1.));
#13661=DIRECTION('',(2.97020476879948E-17,0.970142500145332,-0.242535625036333));
#13662=DIRECTION('center_axis',(0.,-1.,0.));
#13663=DIRECTION('ref_axis',(0.,0.,-1.));
#13664=DIRECTION('center_axis',(0.,-1.,0.));
#13665=DIRECTION('ref_axis',(0.,0.,-1.));
#13666=DIRECTION('center_axis',(0.,-1.,0.));
#13667=DIRECTION('ref_axis',(0.,0.,-1.));
#13668=DIRECTION('center_axis',(0.,-1.,0.));
#13669=DIRECTION('ref_axis',(0.,0.,-1.));
#13670=DIRECTION('',(0.,-1.,0.));
#13671=DIRECTION('center_axis',(0.,-1.,0.));
#13672=DIRECTION('ref_axis',(0.,0.,-1.));
#13673=DIRECTION('center_axis',(0.,1.,0.));
#13674=DIRECTION('ref_axis',(0.,0.,1.));
#13675=DIRECTION('center_axis',(0.,-1.,0.));
#13676=DIRECTION('ref_axis',(0.,0.,-1.));
#13677=DIRECTION('center_axis',(0.,-1.,0.));
#13678=DIRECTION('ref_axis',(0.,0.,-1.));
#13679=DIRECTION('',(0.,-1.,0.));
#13680=DIRECTION('center_axis',(0.,-1.,0.));
#13681=DIRECTION('ref_axis',(0.,0.,-1.));
#13682=DIRECTION('center_axis',(0.,-1.,0.));
#13683=DIRECTION('ref_axis',(0.,0.,-1.));
#13684=DIRECTION('center_axis',(0.,1.,0.));
#13685=DIRECTION('ref_axis',(0.,0.,1.));
#13686=DIRECTION('center_axis',(0.,-1.,0.));
#13687=DIRECTION('ref_axis',(0.,0.,-1.));
#13688=DIRECTION('center_axis',(0.,-1.,0.));
#13689=DIRECTION('ref_axis',(0.,0.,-1.));
#13690=DIRECTION('',(-8.65956056235495E-17,0.707106781186546,-0.707106781186549));
#13691=DIRECTION('center_axis',(0.,-1.,0.));
#13692=DIRECTION('ref_axis',(0.,0.,-1.));
#13693=DIRECTION('',(0.,-1.,0.));
#13694=DIRECTION('center_axis',(0.,-1.,0.));
#13695=DIRECTION('ref_axis',(0.,0.,-1.));
#13696=DIRECTION('center_axis',(0.,-1.,0.));
#13697=DIRECTION('ref_axis',(0.,0.,-1.));
#13698=DIRECTION('center_axis',(0.,1.,0.));
#13699=DIRECTION('ref_axis',(0.,0.,1.));
#13700=DIRECTION('center_axis',(0.,-1.,0.));
#13701=DIRECTION('ref_axis',(0.,0.,-1.));
#13702=DIRECTION('center_axis',(0.,-1.,0.));
#13703=DIRECTION('ref_axis',(0.,0.,-1.));
#13704=DIRECTION('',(-9.10089931823811E-17,0.669130606358856,-0.743144825477396));
#13705=DIRECTION('center_axis',(0.,-1.,0.));
#13706=DIRECTION('ref_axis',(0.,0.,-1.));
#13707=DIRECTION('',(0.,-1.,0.));
#13708=DIRECTION('center_axis',(0.,-1.,0.));
#13709=DIRECTION('ref_axis',(0.,0.,-1.));
#13710=DIRECTION('center_axis',(0.,1.,0.));
#13711=DIRECTION('ref_axis',(0.,0.,1.));
#13712=DIRECTION('center_axis',(0.,-1.,0.));
#13713=DIRECTION('ref_axis',(0.,0.,-1.));
#13714=DIRECTION('center_axis',(0.,-1.,0.));
#13715=DIRECTION('ref_axis',(0.,0.,-1.));
#13716=DIRECTION('',(0.,-1.,0.));
#13717=DIRECTION('axis',(0.,0.,1.));
#13718=DIRECTION('refdir',(1.,0.,0.));
#13719=DIRECTION('center_axis',(-1.,1.11022302462515E-16,6.12323399573677E-17));
#13720=DIRECTION('ref_axis',(0.,0.,1.));
#13721=DIRECTION('center_axis',(-1.11022302462515E-16,-1.,1.22464679914735E-16));
#13722=DIRECTION('ref_axis',(-1.35963107344689E-32,-1.22464679914735E-16,
-1.));
#13723=DIRECTION('',(0.,0.,1.));
#13724=DIRECTION('',(1.,0.,0.));
#13725=DIRECTION('',(0.,0.,1.));
#13726=DIRECTION('',(1.,0.,0.));
#13727=DIRECTION('',(0.,0.,1.));
#13728=DIRECTION('',(1.,0.,0.));
#13729=DIRECTION('',(0.,-1.,0.));
#13730=DIRECTION('',(1.,0.,0.));
#13731=DIRECTION('',(0.,-1.,-2.77555756156289E-17));
#13732=DIRECTION('',(1.,8.80383098281685E-295,-3.17191439469174E-278));
#13733=DIRECTION('',(0.,0.,1.));
#13734=DIRECTION('',(0.309016994374945,0.951056516295155,0.));
#13735=DIRECTION('',(0.,0.,1.));
#13736=DIRECTION('',(-0.809016994374951,0.587785252292469,0.));
#13737=DIRECTION('',(0.,0.,1.));
#13738=DIRECTION('',(-0.809016994374942,-0.58778525229248,0.));
#13739=DIRECTION('',(0.,0.,1.));
#13740=DIRECTION('',(0.309016994374958,-0.95105651629515,0.));
#13741=DIRECTION('axis',(0.,0.,1.));
#13742=DIRECTION('refdir',(1.,0.,0.));
#13743=DIRECTION('center_axis',(0.,-1.,0.));
#13744=DIRECTION('ref_axis',(0.,0.,-1.));
#13745=DIRECTION('center_axis',(0.,-1.,0.));
#13746=DIRECTION('ref_axis',(0.,0.,-1.));
#13747=DIRECTION('center_axis',(0.,-1.,0.));
#13748=DIRECTION('ref_axis',(0.,0.,-1.));
#13749=DIRECTION('center_axis',(0.,-1.,0.));
#13750=DIRECTION('ref_axis',(0.,0.,-1.));
#13751=DIRECTION('',(1.19837786199035E-16,0.206010481049842,-0.978549784986749));
#13752=DIRECTION('center_axis',(0.,-1.,0.));
#13753=DIRECTION('ref_axis',(0.,0.,-1.));
#13754=DIRECTION('center_axis',(0.,1.,0.));
#13755=DIRECTION('ref_axis',(0.,0.,1.));
#13756=DIRECTION('center_axis',(0.,1.,0.));
#13757=DIRECTION('ref_axis',(0.,0.,1.));
#13758=DIRECTION('',(0.,1.,0.));
#13759=DIRECTION('center_axis',(0.,1.,0.));
#13760=DIRECTION('ref_axis',(0.,0.,1.));
#13761=DIRECTION('center_axis',(0.,-1.,0.));
#13762=DIRECTION('ref_axis',(0.,0.,1.));
#13763=DIRECTION('center_axis',(0.,-1.,0.));
#13764=DIRECTION('ref_axis',(0.,0.,-1.));
#13765=DIRECTION('center_axis',(0.,-1.,0.));
#13766=DIRECTION('ref_axis',(0.,0.,-1.));
#13767=DIRECTION('center_axis',(0.,1.,0.));
#13768=DIRECTION('ref_axis',(0.,0.,1.));
#13769=DIRECTION('center_axis',(0.,1.,0.));
#13770=DIRECTION('ref_axis',(0.,0.,1.));
#13771=DIRECTION('',(0.,1.,0.));
#13772=DIRECTION('center_axis',(0.,1.,0.));
#13773=DIRECTION('ref_axis',(0.,0.,1.));
#13774=DIRECTION('',(8.65956056235484E-17,-0.707106781186555,0.70710678118654));
#13775=DIRECTION('center_axis',(0.,1.,0.));
#13776=DIRECTION('ref_axis',(0.,0.,1.));
#13777=DIRECTION('',(8.65956056235494E-17,-0.707106781186547,0.707106781186548));
#13778=DIRECTION('center_axis',(0.,1.,0.));
#13779=DIRECTION('ref_axis',(0.,0.,1.));
#13780=DIRECTION('center_axis',(0.,-1.,0.));
#13781=DIRECTION('ref_axis',(0.,0.,-1.));
#13782=DIRECTION('center_axis',(0.,-1.,0.));
#13783=DIRECTION('ref_axis',(0.,0.,-1.));
#13784=DIRECTION('center_axis',(0.,-1.,0.));
#13785=DIRECTION('ref_axis',(0.,0.,-1.));
#13786=DIRECTION('',(0.,-1.,0.));
#13787=DIRECTION('center_axis',(0.,-1.,0.));
#13788=DIRECTION('ref_axis',(0.,0.,1.));
#13789=DIRECTION('center_axis',(0.,-1.,0.));
#13790=DIRECTION('ref_axis',(0.,0.,-1.));
#13791=DIRECTION('',(-8.65956056235497E-17,-0.707106781186545,0.707106781186551));
#13792=DIRECTION('center_axis',(0.,1.,0.));
#13793=DIRECTION('ref_axis',(0.,0.,1.));
#13794=DIRECTION('center_axis',(0.,1.,0.));
#13795=DIRECTION('ref_axis',(0.,0.,1.));
#13796=DIRECTION('axis',(0.,0.,1.));
#13797=DIRECTION('refdir',(1.,0.,0.));
#13798=DIRECTION('center_axis',(0.,1.,0.));
#13799=DIRECTION('ref_axis',(0.,0.,1.));
#13800=DIRECTION('center_axis',(-1.,0.,1.22464679914735E-16));
#13801=DIRECTION('ref_axis',(-1.22464679914735E-16,0.,-1.));
#13802=DIRECTION('center_axis',(0.,-1.,0.));
#13803=DIRECTION('ref_axis',(0.,0.,1.));
#13804=DIRECTION('axis',(0.,0.,1.));
#13805=DIRECTION('refdir',(1.,0.,0.));
#13806=DIRECTION('center_axis',(0.,1.,0.));
#13807=DIRECTION('ref_axis',(0.,0.,1.));
#13808=DIRECTION('',(0.866025403784438,0.,0.5));
#13809=DIRECTION('center_axis',(0.,-1.,0.));
#13810=DIRECTION('ref_axis',(0.,0.,1.));
#13811=DIRECTION('',(1.1556266144132E-16,0.,1.));
#13812=DIRECTION('center_axis',(0.,-1.,0.));
#13813=DIRECTION('ref_axis',(0.,0.,1.));
#13814=DIRECTION('',(-0.866025403784439,0.,0.5));
#13815=DIRECTION('center_axis',(0.,-1.,0.));
#13816=DIRECTION('ref_axis',(0.,0.,1.));
#13817=DIRECTION('',(-0.866025403784438,0.,-0.5));
#13818=DIRECTION('center_axis',(0.,-1.,0.));
#13819=DIRECTION('ref_axis',(-8.88178419700125E-16,0.,1.));
#13820=DIRECTION('',(-1.1556266144132E-16,0.,-1.));
#13821=DIRECTION('center_axis',(0.,-1.,0.));
#13822=DIRECTION('ref_axis',(-8.88178419700125E-16,0.,1.));
#13823=DIRECTION('',(0.866025403784439,0.,-0.5));
#13824=DIRECTION('center_axis',(0.,-1.,0.));
#13825=DIRECTION('ref_axis',(0.,0.,1.));
#13826=DIRECTION('center_axis',(0.,-1.,0.));
#13827=DIRECTION('ref_axis',(0.,0.,-1.));
#13828=DIRECTION('center_axis',(0.,1.,0.));
#13829=DIRECTION('ref_axis',(0.,0.,1.));
#13830=DIRECTION('center_axis',(0.,-1.,0.));
#13831=DIRECTION('ref_axis',(0.,0.,1.));
#13832=DIRECTION('',(0.866025403784438,0.,0.5));
#13833=DIRECTION('center_axis',(0.,-1.,0.));
#13834=DIRECTION('ref_axis',(0.,0.,1.));
#13835=DIRECTION('',(0.866025403784439,0.,-0.5));
#13836=DIRECTION('center_axis',(0.,-1.,0.));
#13837=DIRECTION('ref_axis',(-8.88178419700125E-16,0.,1.));
#13838=DIRECTION('',(-1.1556266144132E-16,0.,-1.));
#13839=DIRECTION('center_axis',(0.,-1.,0.));
#13840=DIRECTION('ref_axis',(-8.88178419700125E-16,0.,1.));
#13841=DIRECTION('',(-0.866025403784438,0.,-0.5));
#13842=DIRECTION('center_axis',(0.,-1.,0.));
#13843=DIRECTION('ref_axis',(0.,0.,1.));
#13844=DIRECTION('',(-0.866025403784439,0.,0.5));
#13845=DIRECTION('center_axis',(0.,-1.,0.));
#13846=DIRECTION('ref_axis',(0.,0.,1.));
#13847=DIRECTION('',(1.1556266144132E-16,0.,1.));
#13848=DIRECTION('center_axis',(0.,1.,0.));
#13849=DIRECTION('ref_axis',(0.,0.,1.));
#13850=DIRECTION('center_axis',(-1.,0.,1.1556266144132E-16));
#13851=DIRECTION('ref_axis',(1.1556266144132E-16,0.,1.));
#13852=DIRECTION('',(0.,-1.,0.));
#13853=DIRECTION('',(0.,-1.,0.));
#13854=DIRECTION('center_axis',(-0.5,0.,0.866025403784439));
#13855=DIRECTION('ref_axis',(0.866025403784439,0.,0.5));
#13856=DIRECTION('',(0.,-1.,0.));
#13857=DIRECTION('center_axis',(0.5,0.,0.866025403784439));
#13858=DIRECTION('ref_axis',(0.866025403784439,0.,-0.5));
#13859=DIRECTION('',(0.,-1.,0.));
#13860=DIRECTION('center_axis',(1.,0.,-1.1556266144132E-16));
#13861=DIRECTION('ref_axis',(-1.1556266144132E-16,0.,-1.));
#13862=DIRECTION('',(0.,-1.,0.));
#13863=DIRECTION('center_axis',(0.5,0.,-0.866025403784439));
#13864=DIRECTION('ref_axis',(-0.866025403784439,0.,-0.5));
#13865=DIRECTION('',(0.,-1.,0.));
#13866=DIRECTION('center_axis',(-0.5,0.,-0.866025403784439));
#13867=DIRECTION('ref_axis',(-0.866025403784439,0.,0.5));
#13868=DIRECTION('center_axis',(0.,-1.,0.));
#13869=DIRECTION('ref_axis',(1.89882151931499E-15,0.,1.));
#13870=DIRECTION('center_axis',(0.,-1.,0.));
#13871=DIRECTION('ref_axis',(0.,0.,-1.));
#13872=DIRECTION('center_axis',(0.,-1.,0.));
#13873=DIRECTION('ref_axis',(0.,0.,-1.));
#13874=DIRECTION('center_axis',(0.,-1.,0.));
#13875=DIRECTION('ref_axis',(0.,0.,-1.));
#13876=DIRECTION('center_axis',(0.,-1.,0.));
#13877=DIRECTION('ref_axis',(0.,0.,-1.));
#13878=DIRECTION('center_axis',(0.,-1.,0.));
#13879=DIRECTION('ref_axis',(0.,0.,-1.));
#13880=DIRECTION('center_axis',(0.,1.,0.));
#13881=DIRECTION('ref_axis',(2.9861597890357E-15,0.,1.));
#13882=DIRECTION('center_axis',(0.,1.,0.));
#13883=DIRECTION('ref_axis',(0.,0.,-1.));
#13884=DIRECTION('center_axis',(0.,1.,0.));
#13885=DIRECTION('ref_axis',(0.,0.,-1.));
#13886=DIRECTION('center_axis',(0.,1.,0.));
#13887=DIRECTION('ref_axis',(0.,0.,-1.));
#13888=DIRECTION('center_axis',(0.,1.,0.));
#13889=DIRECTION('ref_axis',(0.,0.,-1.));
#13890=DIRECTION('center_axis',(0.,1.,0.));
#13891=DIRECTION('ref_axis',(0.,0.,-1.));
#13892=DIRECTION('center_axis',(0.,-1.,0.));
#13893=DIRECTION('ref_axis',(0.,0.,-1.));
#13894=DIRECTION('',(0.,-1.,0.));
#13895=DIRECTION('',(5.55111512312578E-17,0.,1.));
#13896=DIRECTION('',(-1.,0.,5.55111512312578E-17));
#13897=DIRECTION('',(0.,0.,1.));
#13898=DIRECTION('',(1.,0.,0.));
#13899=DIRECTION('',(2.38406900122897E-36,-1.,1.15555796663234E-32));
#13900=DIRECTION('',(1.,2.38406900122833E-36,-5.55111512312577E-17));
#13901=DIRECTION('',(0.,0.,1.));
#13902=DIRECTION('',(1.,0.,0.));
#13903=DIRECTION('',(0.,0.,1.));
#13904=DIRECTION('',(1.,0.,0.));
#13905=DIRECTION('',(0.,0.,1.));
#13906=DIRECTION('',(-1.,-1.22464679914735E-16,0.));
#13907=DIRECTION('',(-1.22464679914735E-16,1.,3.97989445980249E-48));
#13908=DIRECTION('',(-1.,-1.22464679914735E-16,6.27599107403457E-32));
#13909=DIRECTION('',(1.11022302462516E-16,-1.,0.));
#13910=DIRECTION('',(-1.,-1.11022302462516E-16,0.));
#13911=DIRECTION('',(1.11022302462516E-16,-1.,-1.54074395550979E-33));
#13912=DIRECTION('',(1.,1.11022302462516E-16,1.36663352413238E-15));
#13913=DIRECTION('',(-1.11022302462516E-16,-1.,2.65460481607669E-20));
#13914=DIRECTION('',(1.,-1.11022302462516E-16,-5.5440277913215E-17));
#13915=CARTESIAN_POINT('',(0.,0.,0.));
#13916=CARTESIAN_POINT('',(0.,0.,0.));
#13917=CARTESIAN_POINT('Origin',(0.,10.75,0.));
#13918=CARTESIAN_POINT('',(-4.19956186204517,10.7500000000001,17.503247703408));
#13919=CARTESIAN_POINT('',(-4.19956186204517,-5.74999999999987,17.503247703408));
#13920=CARTESIAN_POINT('',(-4.19956186204517,333.257395605323,17.503247703408));
#13921=CARTESIAN_POINT('',(-4.20447115411988,-5.75,17.5020690866587));
#13922=CARTESIAN_POINT('Origin',(0.,-5.75,0.));
#13923=CARTESIAN_POINT('',(-4.20447115411988,10.7500000000001,17.5020690866587));
#13924=CARTESIAN_POINT('',(-4.20447115411988,333.257395605323,17.5020690866587));
#13925=CARTESIAN_POINT('Origin',(0.,10.75,0.));
#13926=CARTESIAN_POINT('Origin',(0.,10.75,0.));
#13927=CARTESIAN_POINT('',(-6.8859694776993,10.7500000000001,16.6307974659123));
#13928=CARTESIAN_POINT('',(-6.88596947769931,-5.74999999999998,16.6307974659123));
#13929=CARTESIAN_POINT('',(-6.8859694776993,333.257395605323,16.6307974659123));
#13930=CARTESIAN_POINT('',(-6.8906339519614,-5.75,16.6288653774116));
#13931=CARTESIAN_POINT('Origin',(0.,-5.75,0.));
#13932=CARTESIAN_POINT('',(-6.8906339519614,10.7500000000001,16.6288653774116));
#13933=CARTESIAN_POINT('',(-6.8906339519614,333.257395605323,16.6288653774116));
#13934=CARTESIAN_POINT('Origin',(0.,10.75,0.));
#13935=CARTESIAN_POINT('Origin',(0.,10.75,0.));
#13936=CARTESIAN_POINT('',(-9.40282167159,10.7500000000001,15.3488418003535));
#13937=CARTESIAN_POINT('',(-9.40282167159,-5.74999999999998,15.3488418003535));
#13938=CARTESIAN_POINT('',(-9.40282167159,333.257395605323,15.3488418003535));
#13939=CARTESIAN_POINT('',(-9.40712647320266,-5.75,15.3462038145324));
#13940=CARTESIAN_POINT('Origin',(0.,-5.75,0.));
#13941=CARTESIAN_POINT('',(-9.40712647320266,10.7500000000001,15.3462038145324));
#13942=CARTESIAN_POINT('',(-9.40712647320266,333.257395605323,15.3462038145324));
#13943=CARTESIAN_POINT('Origin',(0.,10.75,0.));
#13944=CARTESIAN_POINT('Origin',(0.,10.75,0.));
#13945=CARTESIAN_POINT('',(-11.6881451897502,10.7500000000001,13.6889467097845));
#13946=CARTESIAN_POINT('',(-11.6881451897502,-5.74999999999998,13.6889467097845));
#13947=CARTESIAN_POINT('',(-11.6881451897502,333.257395605323,13.6889467097845));
#13948=CARTESIAN_POINT('',(-11.6919843202109,-5.75,13.685667782609));
#13949=CARTESIAN_POINT('Origin',(0.,-5.75,0.));
#13950=CARTESIAN_POINT('',(-11.6919843202109,10.7500000000001,13.685667782609));
#13951=CARTESIAN_POINT('',(-11.6919843202109,333.257395605323,13.685667782609));
#13952=CARTESIAN_POINT('Origin',(0.,10.75,0.));
#13953=CARTESIAN_POINT('Origin',(0.,10.75,0.));
#13954=CARTESIAN_POINT('',(-13.6856677826088,10.7500000000001,11.6919843202112));
#13955=CARTESIAN_POINT('',(-13.6856677826088,-5.74999999999998,11.6919843202112));
#13956=CARTESIAN_POINT('',(-13.6856677826088,333.257395605323,11.6919843202112));
#13957=CARTESIAN_POINT('',(-13.6889467097842,-5.75,11.6881451897505));
#13958=CARTESIAN_POINT('Origin',(0.,-5.75,0.));
#13959=CARTESIAN_POINT('',(-13.6889467097842,10.7500000000001,11.6881451897505));
#13960=CARTESIAN_POINT('',(-13.6889467097842,333.257395605323,11.6881451897505));
#13961=CARTESIAN_POINT('Origin',(0.,10.75,0.));
#13962=CARTESIAN_POINT('Origin',(0.,10.75,0.));
#13963=CARTESIAN_POINT('',(-15.3462038145322,10.7500000000001,9.40712647320306));
#13964=CARTESIAN_POINT('',(-15.3462038145322,-5.74999999999998,9.40712647320306));
#13965=CARTESIAN_POINT('',(-15.3462038145322,333.257395605323,9.40712647320306));
#13966=CARTESIAN_POINT('',(-15.3488418003532,-5.75,9.40282167159038));
#13967=CARTESIAN_POINT('Origin',(0.,-5.75,0.));
#13968=CARTESIAN_POINT('',(-15.3488418003532,10.7500000000001,9.40282167159038));
#13969=CARTESIAN_POINT('',(-15.3488418003532,333.257395605323,9.40282167159038));
#13970=CARTESIAN_POINT('Origin',(0.,10.75,0.));
#13971=CARTESIAN_POINT('Origin',(0.,10.75,0.));
#13972=CARTESIAN_POINT('',(-16.6288653774114,10.7500000000001,6.89063395196181));
#13973=CARTESIAN_POINT('',(-16.6288653774114,-5.74999999999998,6.89063395196181));
#13974=CARTESIAN_POINT('',(-16.6288653774114,333.257395605323,6.89063395196181));
#13975=CARTESIAN_POINT('',(-16.6307974659121,-5.75,6.88596947769972));
#13976=CARTESIAN_POINT('Origin',(0.,-5.75,0.));
#13977=CARTESIAN_POINT('',(-16.6307974659121,10.7500000000001,6.88596947769972));
#13978=CARTESIAN_POINT('',(-16.6307974659121,333.257395605323,6.88596947769972));
#13979=CARTESIAN_POINT('Origin',(0.,10.75,0.));
#13980=CARTESIAN_POINT('Origin',(0.,10.75,0.));
#13981=CARTESIAN_POINT('',(-17.5020690866586,10.7500000000001,4.20447115412031));
#13982=CARTESIAN_POINT('',(-17.5020690866586,-5.74999999999998,4.20447115412031));
#13983=CARTESIAN_POINT('',(-17.5020690866586,333.257395605323,4.20447115412031));
#13984=CARTESIAN_POINT('',(-17.5032477034078,-5.75,4.19956186204562));
#13985=CARTESIAN_POINT('Origin',(0.,-5.75,0.));
#13986=CARTESIAN_POINT('',(-17.5032477034078,10.7500000000001,4.19956186204562));
#13987=CARTESIAN_POINT('',(-17.5032477034078,333.257395605323,4.19956186204562));
#13988=CARTESIAN_POINT('Origin',(0.,10.75,0.));
#13989=CARTESIAN_POINT('Origin',(0.,10.75,0.));
#13990=CARTESIAN_POINT('',(-17.9443137689552,10.7500000000001,1.41478032262462));
#13991=CARTESIAN_POINT('',(-17.9443137689552,-5.74999999999998,1.41478032262462));
#13992=CARTESIAN_POINT('',(-17.9443137689552,333.257395605323,1.41478032262462));
#13993=CARTESIAN_POINT('',(-17.944709892497,-5.75,1.40974709580119));
#13994=CARTESIAN_POINT('Origin',(0.,-5.75,0.));
#13995=CARTESIAN_POINT('',(-17.944709892497,10.7500000000001,1.40974709580119));
#13996=CARTESIAN_POINT('',(-17.944709892497,333.257395605323,1.40974709580119));
#13997=CARTESIAN_POINT('Origin',(0.,10.75,0.));
#13998=CARTESIAN_POINT('Origin',(0.,10.75,0.));
#13999=CARTESIAN_POINT('',(-17.944709892497,10.7500000000001,-1.40974709580081));
#14000=CARTESIAN_POINT('',(-17.944709892497,-5.74999999999998,-1.40974709580081));
#14001=CARTESIAN_POINT('',(-17.944709892497,333.257395605323,-1.40974709580081));
#14002=CARTESIAN_POINT('',(-17.9443137689552,-5.75,-1.41478032262422));
#14003=CARTESIAN_POINT('Origin',(0.,-5.75,0.));
#14004=CARTESIAN_POINT('',(-17.9443137689552,10.7500000000001,-1.41478032262422));
#14005=CARTESIAN_POINT('',(-17.9443137689552,333.257395605323,-1.41478032262422));
#14006=CARTESIAN_POINT('Origin',(0.,10.75,0.));
#14007=CARTESIAN_POINT('Origin',(0.,10.75,0.));
#14008=CARTESIAN_POINT('',(-17.5032477034079,10.7500000000001,-4.19956186204523));
#14009=CARTESIAN_POINT('',(-17.5032477034079,-5.74999999999998,-4.19956186204523));
#14010=CARTESIAN_POINT('',(-17.5032477034079,333.257395605323,-4.19956186204523));
#14011=CARTESIAN_POINT('',(-17.5020690866587,-5.75,-4.20447115411994));
#14012=CARTESIAN_POINT('Origin',(0.,-5.75,0.));
#14013=CARTESIAN_POINT('',(-17.5020690866587,10.7500000000001,-4.20447115411994));
#14014=CARTESIAN_POINT('',(-17.5020690866587,333.257395605323,-4.20447115411994));
#14015=CARTESIAN_POINT('Origin',(0.,10.75,0.));
#14016=CARTESIAN_POINT('Origin',(0.,10.75,0.));
#14017=CARTESIAN_POINT('',(-16.6307974659122,10.7500000000001,-6.88596947769936));
#14018=CARTESIAN_POINT('',(-16.6307974659122,-5.74999999999998,-6.88596947769936));
#14019=CARTESIAN_POINT('',(-16.6307974659122,333.257395605323,-6.88596947769936));
#14020=CARTESIAN_POINT('',(-16.6288653774115,-5.75,-6.89063395196146));
#14021=CARTESIAN_POINT('Origin',(0.,-5.75,0.));
#14022=CARTESIAN_POINT('',(-16.6288653774115,10.7500000000001,-6.89063395196146));
#14023=CARTESIAN_POINT('',(-16.6288653774115,333.257395605323,-6.89063395196146));
#14024=CARTESIAN_POINT('Origin',(0.,10.75,0.));
#14025=CARTESIAN_POINT('Origin',(0.,10.75,0.));
#14026=CARTESIAN_POINT('',(-15.3488418003534,10.7500000000001,-9.40282167159006));
#14027=CARTESIAN_POINT('',(-15.3488418003534,-5.74999999999998,-9.40282167159006));
#14028=CARTESIAN_POINT('',(-15.3488418003534,333.257395605323,-9.40282167159006));
#14029=CARTESIAN_POINT('',(-15.3462038145324,-5.75,-9.40712647320272));
#14030=CARTESIAN_POINT('Origin',(0.,-5.75,0.));
#14031=CARTESIAN_POINT('',(-15.3462038145324,10.7500000000001,-9.40712647320272));
#14032=CARTESIAN_POINT('',(-15.3462038145324,333.257395605323,-9.40712647320272));
#14033=CARTESIAN_POINT('Origin',(0.,10.75,0.));
#14034=CARTESIAN_POINT('Origin',(0.,10.75,0.));
#14035=CARTESIAN_POINT('',(-13.6889467097845,10.7500000000001,-11.6881451897502));
#14036=CARTESIAN_POINT('',(-13.6889467097845,-5.74999999999998,-11.6881451897502));
#14037=CARTESIAN_POINT('',(-13.6889467097845,333.257395605323,-11.6881451897502));
#14038=CARTESIAN_POINT('',(-13.685667782609,-5.74999999999998,-11.6919843202109));
#14039=CARTESIAN_POINT('Origin',(0.,-5.75,0.));
#14040=CARTESIAN_POINT('',(-13.685667782609,10.7500000000001,-11.6919843202109));
#14041=CARTESIAN_POINT('',(-13.685667782609,333.257395605323,-11.6919843202109));
#14042=CARTESIAN_POINT('Origin',(0.,10.75,0.));
#14043=CARTESIAN_POINT('Origin',(0.,10.75,0.));
#14044=CARTESIAN_POINT('',(-11.6919843202112,10.7500000000001,-13.6856677826088));
#14045=CARTESIAN_POINT('',(-11.6919843202112,-5.75,-13.6856677826088));
#14046=CARTESIAN_POINT('',(-11.6919843202112,333.257395605323,-13.6856677826088));
#14047=CARTESIAN_POINT('',(-11.6881451897505,-5.74999999999998,-13.6889467097843));
#14048=CARTESIAN_POINT('Origin',(0.,-5.75,0.));
#14049=CARTESIAN_POINT('',(-11.6881451897505,10.7500000000001,-13.6889467097843));
#14050=CARTESIAN_POINT('',(-11.6881451897505,333.257395605323,-13.6889467097843));
#14051=CARTESIAN_POINT('Origin',(0.,10.75,0.));
#14052=CARTESIAN_POINT('Origin',(0.,10.75,0.));
#14053=CARTESIAN_POINT('',(-9.40712647320301,10.7500000000001,-15.3462038145322));
#14054=CARTESIAN_POINT('',(-9.40712647320301,-5.75,-15.3462038145322));
#14055=CARTESIAN_POINT('',(-9.40712647320301,333.257395605323,-15.3462038145322));
#14056=CARTESIAN_POINT('',(-9.40282167159034,-5.74999999999998,-15.3488418003532));
#14057=CARTESIAN_POINT('Origin',(0.,-5.75,0.));
#14058=CARTESIAN_POINT('',(-9.40282167159034,10.7500000000001,-15.3488418003532));
#14059=CARTESIAN_POINT('',(-9.40282167159034,333.257395605323,-15.3488418003532));
#14060=CARTESIAN_POINT('Origin',(0.,10.75,0.));
#14061=CARTESIAN_POINT('Origin',(0.,10.75,0.));
#14062=CARTESIAN_POINT('',(-6.89063395196176,10.7500000000001,-16.6288653774114));
#14063=CARTESIAN_POINT('',(-6.89063395196176,-5.75,-16.6288653774114));
#14064=CARTESIAN_POINT('',(-6.89063395196176,333.257395605323,-16.6288653774114));
#14065=CARTESIAN_POINT('',(-6.88596947769966,-5.74999999999998,-16.6307974659121));
#14066=CARTESIAN_POINT('Origin',(0.,-5.75,0.));
#14067=CARTESIAN_POINT('',(-6.88596947769966,10.7500000000001,-16.6307974659121));
#14068=CARTESIAN_POINT('',(-6.88596947769966,333.257395605323,-16.6307974659121));
#14069=CARTESIAN_POINT('Origin',(0.,10.75,0.));
#14070=CARTESIAN_POINT('Origin',(0.,10.75,0.));
#14071=CARTESIAN_POINT('',(-4.20447115412025,10.7500000000001,-17.5020690866586));
#14072=CARTESIAN_POINT('',(-4.20447115412025,-5.75,-17.5020690866586));
#14073=CARTESIAN_POINT('',(-4.20447115412025,333.257395605323,-17.5020690866586));
#14074=CARTESIAN_POINT('',(-4.19956186204555,-5.74999999999998,-17.5032477034079));
#14075=CARTESIAN_POINT('Origin',(0.,-5.75,0.));
#14076=CARTESIAN_POINT('',(-4.19956186204555,10.7500000000001,-17.5032477034079));
#14077=CARTESIAN_POINT('',(-4.19956186204555,333.257395605323,-17.5032477034079));
#14078=CARTESIAN_POINT('Origin',(0.,10.75,0.));
#14079=CARTESIAN_POINT('Origin',(0.,10.75,0.));
#14080=CARTESIAN_POINT('',(-1.41478032262455,10.7500000000001,-17.9443137689552));
#14081=CARTESIAN_POINT('',(-1.41478032262455,-5.75,-17.9443137689552));
#14082=CARTESIAN_POINT('',(-1.41478032262455,333.257395605323,-17.9443137689552));
#14083=CARTESIAN_POINT('',(-1.409747095801,-5.74999999999998,-17.944709892497));
#14084=CARTESIAN_POINT('Origin',(0.,-5.75,0.));
#14085=CARTESIAN_POINT('',(-1.409747095801,10.7500000000001,-17.944709892497));
#14086=CARTESIAN_POINT('',(-1.409747095801,333.257395605323,-17.944709892497));
#14087=CARTESIAN_POINT('Origin',(0.,10.75,0.));
#14088=CARTESIAN_POINT('Origin',(0.,10.75,0.));
#14089=CARTESIAN_POINT('',(1.40974709580099,10.7500000000001,-17.944709892497));
#14090=CARTESIAN_POINT('',(1.40974709580099,-5.75,-17.944709892497));
#14091=CARTESIAN_POINT('',(1.40974709580099,333.257395605323,-17.944709892497));
#14092=CARTESIAN_POINT('',(1.41478032262429,-5.74999999999998,-17.9443137689552));
#14093=CARTESIAN_POINT('Origin',(0.,-5.75,0.));
#14094=CARTESIAN_POINT('',(1.41478032262429,10.7500000000001,-17.9443137689552));
#14095=CARTESIAN_POINT('',(1.41478032262429,333.257395605323,-17.9443137689552));
#14096=CARTESIAN_POINT('Origin',(0.,10.75,0.));
#14097=CARTESIAN_POINT('Origin',(0.,10.75,0.));
#14098=CARTESIAN_POINT('',(4.1995618620453,10.7500000000001,-17.5032477034079));
#14099=CARTESIAN_POINT('',(4.19956186204529,-5.75,-17.5032477034079));
#14100=CARTESIAN_POINT('',(4.1995618620453,333.257395605323,-17.5032477034079));
#14101=CARTESIAN_POINT('',(4.20447115411999,-5.74999999999998,-17.5020690866587));
#14102=CARTESIAN_POINT('Origin',(0.,-5.75,0.));
#14103=CARTESIAN_POINT('',(4.20447115411999,10.7500000000001,-17.5020690866587));
#14104=CARTESIAN_POINT('',(4.20447115411999,333.257395605323,-17.5020690866587));
#14105=CARTESIAN_POINT('Origin',(0.,10.75,0.));
#14106=CARTESIAN_POINT('Origin',(0.,10.75,0.));
#14107=CARTESIAN_POINT('',(6.88596947769941,10.7500000000001,-16.6307974659122));
#14108=CARTESIAN_POINT('',(6.88596947769941,-5.75,-16.6307974659122));
#14109=CARTESIAN_POINT('',(6.88596947769941,333.257395605323,-16.6307974659122));
#14110=CARTESIAN_POINT('',(6.89063395196152,-5.74999999999998,-16.6288653774115));
#14111=CARTESIAN_POINT('Origin',(0.,-5.75,0.));
#14112=CARTESIAN_POINT('',(6.89063395196152,10.7500000000001,-16.6288653774115));
#14113=CARTESIAN_POINT('',(6.89063395196152,333.257395605323,-16.6288653774115));
#14114=CARTESIAN_POINT('Origin',(0.,10.75,0.));
#14115=CARTESIAN_POINT('Origin',(0.,10.75,0.));
#14116=CARTESIAN_POINT('',(9.40282167159011,10.7500000000001,-15.3488418003534));
#14117=CARTESIAN_POINT('',(9.40282167159011,-5.75,-15.3488418003534));
#14118=CARTESIAN_POINT('',(9.40282167159011,333.257395605323,-15.3488418003534));
#14119=CARTESIAN_POINT('',(9.40712647320278,-5.74999999999998,-15.3462038145324));
#14120=CARTESIAN_POINT('Origin',(0.,-5.75,0.));
#14121=CARTESIAN_POINT('',(9.40712647320278,10.7500000000001,-15.3462038145324));
#14122=CARTESIAN_POINT('',(9.40712647320278,333.257395605323,-15.3462038145324));
#14123=CARTESIAN_POINT('Origin',(0.,10.75,0.));
#14124=CARTESIAN_POINT('Origin',(0.,10.75,0.));
#14125=CARTESIAN_POINT('',(11.6881451897503,10.7500000000001,-13.6889467097844));
#14126=CARTESIAN_POINT('',(11.6881451897503,-5.75,-13.6889467097844));
#14127=CARTESIAN_POINT('',(11.6881451897503,333.257395605323,-13.6889467097844));
#14128=CARTESIAN_POINT('',(11.691984320211,-5.74999999999998,-13.685667782609));
#14129=CARTESIAN_POINT('Origin',(0.,-5.75,0.));
#14130=CARTESIAN_POINT('',(11.691984320211,10.7500000000001,-13.685667782609));
#14131=CARTESIAN_POINT('',(11.691984320211,333.257395605323,-13.685667782609));
#14132=CARTESIAN_POINT('Origin',(0.,10.75,0.));
#14133=CARTESIAN_POINT('Origin',(0.,10.75,0.));
#14134=CARTESIAN_POINT('',(13.6856677826088,10.7500000000001,-11.6919843202111));
#14135=CARTESIAN_POINT('',(13.6856677826088,-5.75,-11.6919843202111));
#14136=CARTESIAN_POINT('',(13.6856677826088,333.257395605323,-11.6919843202111));
#14137=CARTESIAN_POINT('',(13.6889467097843,-5.74999999999998,-11.6881451897504));
#14138=CARTESIAN_POINT('Origin',(0.,-5.75,0.));
#14139=CARTESIAN_POINT('',(13.6889467097843,10.7500000000001,-11.6881451897504));
#14140=CARTESIAN_POINT('',(13.6889467097843,333.257395605323,-11.6881451897504));
#14141=CARTESIAN_POINT('Origin',(0.,10.75,0.));
#14142=CARTESIAN_POINT('Origin',(0.,10.75,0.));
#14143=CARTESIAN_POINT('',(15.3462038145323,10.7500000000001,-9.40712647320295));
#14144=CARTESIAN_POINT('',(15.3462038145323,-5.75,-9.40712647320295));
#14145=CARTESIAN_POINT('',(15.3462038145323,333.257395605323,-9.40712647320295));
#14146=CARTESIAN_POINT('',(15.3488418003533,-5.74999999999998,-9.40282167159028));
#14147=CARTESIAN_POINT('Origin',(0.,-5.75,0.));
#14148=CARTESIAN_POINT('',(15.3488418003533,10.7500000000001,-9.40282167159028));
#14149=CARTESIAN_POINT('',(15.3488418003533,333.257395605323,-9.40282167159028));
#14150=CARTESIAN_POINT('Origin',(0.,10.75,0.));
#14151=CARTESIAN_POINT('Origin',(0.,10.75,0.));
#14152=CARTESIAN_POINT('',(16.6288653774114,10.7500000000001,-6.8906339519617));
#14153=CARTESIAN_POINT('',(16.6288653774114,-5.75,-6.8906339519617));
#14154=CARTESIAN_POINT('',(16.6288653774114,333.257395605323,-6.8906339519617));
#14155=CARTESIAN_POINT('',(16.6307974659121,-5.74999999999998,-6.8859694776996));
#14156=CARTESIAN_POINT('Origin',(0.,-5.75,0.));
#14157=CARTESIAN_POINT('',(16.6307974659121,10.7500000000001,-6.8859694776996));
#14158=CARTESIAN_POINT('',(16.6307974659121,333.257395605323,-6.8859694776996));
#14159=CARTESIAN_POINT('Origin',(0.,10.75,0.));
#14160=CARTESIAN_POINT('Origin',(0.,10.75,0.));
#14161=CARTESIAN_POINT('',(17.5020690866586,10.7500000000001,-4.20447115412019));
#14162=CARTESIAN_POINT('',(17.5020690866586,-5.75,-4.20447115412019));
#14163=CARTESIAN_POINT('',(17.5020690866586,333.257395605323,-4.20447115412019));
#14164=CARTESIAN_POINT('',(17.5032477034079,-5.74999999999998,-4.19956186204549));
#14165=CARTESIAN_POINT('Origin',(0.,-5.75,0.));
#14166=CARTESIAN_POINT('',(17.5032477034079,10.7500000000001,-4.19956186204549));
#14167=CARTESIAN_POINT('',(17.5032477034079,333.257395605323,-4.19956186204549));
#14168=CARTESIAN_POINT('Origin',(0.,10.75,0.));
#14169=CARTESIAN_POINT('Origin',(0.,10.75,0.));
#14170=CARTESIAN_POINT('',(17.9443137689552,10.7500000000001,-1.41478032262448));
#14171=CARTESIAN_POINT('',(17.9443137689552,-5.75,-1.41478032262448));
#14172=CARTESIAN_POINT('',(17.9443137689552,333.257395605323,-1.41478032262448));
#14173=CARTESIAN_POINT('',(17.944709892497,-5.74999999999998,-1.40974709580106));
#14174=CARTESIAN_POINT('Origin',(0.,-5.75,0.));
#14175=CARTESIAN_POINT('',(17.944709892497,10.7500000000001,-1.40974709580106));
#14176=CARTESIAN_POINT('',(17.944709892497,333.257395605323,-1.40974709580106));
#14177=CARTESIAN_POINT('Origin',(0.,10.75,0.));
#14178=CARTESIAN_POINT('Origin',(0.,10.75,0.));
#14179=CARTESIAN_POINT('',(17.944709892497,10.7500000000001,1.40974709580093));
#14180=CARTESIAN_POINT('',(17.944709892497,-5.75,1.40974709580093));
#14181=CARTESIAN_POINT('',(17.944709892497,333.257395605323,1.40974709580093));
#14182=CARTESIAN_POINT('',(17.9443137689552,-5.74999999999998,1.41478032262435));
#14183=CARTESIAN_POINT('Origin',(0.,-5.75,0.));
#14184=CARTESIAN_POINT('',(17.9443137689552,10.7500000000001,1.41478032262435));
#14185=CARTESIAN_POINT('',(17.9443137689552,333.257395605323,1.41478032262435));
#14186=CARTESIAN_POINT('Origin',(0.,10.75,0.));
#14187=CARTESIAN_POINT('Origin',(0.,10.75,0.));
#14188=CARTESIAN_POINT('',(17.5032477034079,10.7500000000001,4.19956186204535));
#14189=CARTESIAN_POINT('',(17.5032477034079,-5.75,4.19956186204535));
#14190=CARTESIAN_POINT('',(17.5032477034079,333.257395605323,4.19956186204535));
#14191=CARTESIAN_POINT('',(17.5020690866587,-5.74999999999998,4.20447115412006));
#14192=CARTESIAN_POINT('Origin',(0.,-5.75,0.));
#14193=CARTESIAN_POINT('',(17.5020690866587,10.7500000000001,4.20447115412006));
#14194=CARTESIAN_POINT('',(17.5020690866587,333.257395605323,4.20447115412006));
#14195=CARTESIAN_POINT('Origin',(0.,10.75,0.));
#14196=CARTESIAN_POINT('Origin',(0.,10.75,0.));
#14197=CARTESIAN_POINT('',(16.6307974659122,10.7500000000001,6.88596947769947));
#14198=CARTESIAN_POINT('',(16.6307974659122,-5.75,6.88596947769947));
#14199=CARTESIAN_POINT('',(16.6307974659122,333.257395605323,6.88596947769947));
#14200=CARTESIAN_POINT('',(16.6288653774115,-5.74999999999998,6.89063395196158));
#14201=CARTESIAN_POINT('Origin',(0.,-5.75,0.));
#14202=CARTESIAN_POINT('',(16.6288653774115,10.7500000000001,6.89063395196158));
#14203=CARTESIAN_POINT('',(16.6288653774115,333.257395605323,6.89063395196158));
#14204=CARTESIAN_POINT('Origin',(0.,10.75,0.));
#14205=CARTESIAN_POINT('Origin',(0.,10.75,0.));
#14206=CARTESIAN_POINT('',(15.3488418003534,10.7500000000001,9.40282167159017));
#14207=CARTESIAN_POINT('',(15.3488418003534,-5.75,9.40282167159017));
#14208=CARTESIAN_POINT('',(15.3488418003534,333.257395605323,9.40282167159017));
#14209=CARTESIAN_POINT('',(15.3462038145323,-5.74999999999998,9.40712647320283));
#14210=CARTESIAN_POINT('Origin',(0.,-5.75,0.));
#14211=CARTESIAN_POINT('',(15.3462038145323,10.7500000000001,9.40712647320283));
#14212=CARTESIAN_POINT('',(15.3462038145323,333.257395605323,9.40712647320283));
#14213=CARTESIAN_POINT('Origin',(0.,10.75,0.));
#14214=CARTESIAN_POINT('Origin',(0.,10.75,0.));
#14215=CARTESIAN_POINT('',(13.6889467097844,10.7500000000001,11.6881451897503));
#14216=CARTESIAN_POINT('',(13.6889467097844,-5.75,11.6881451897503));
#14217=CARTESIAN_POINT('',(13.6889467097844,333.257395605323,11.6881451897503));
#14218=CARTESIAN_POINT('',(13.6856677826089,-5.74999999999998,11.691984320211));
#14219=CARTESIAN_POINT('Origin',(0.,-5.75,0.));
#14220=CARTESIAN_POINT('',(13.6856677826089,10.7500000000001,11.691984320211));
#14221=CARTESIAN_POINT('',(13.6856677826089,333.257395605323,11.691984320211));
#14222=CARTESIAN_POINT('Origin',(0.,10.75,0.));
#14223=CARTESIAN_POINT('Origin',(0.,10.75,0.));
#14224=CARTESIAN_POINT('',(11.6919843202111,10.7500000000001,13.6856677826089));
#14225=CARTESIAN_POINT('',(11.6919843202111,-5.75,13.6856677826089));
#14226=CARTESIAN_POINT('',(11.6919843202111,333.257395605323,13.6856677826089));
#14227=CARTESIAN_POINT('',(11.6881451897504,-5.74999999999998,13.6889467097843));
#14228=CARTESIAN_POINT('Origin',(0.,-5.75,0.));
#14229=CARTESIAN_POINT('',(11.6881451897504,10.7500000000001,13.6889467097843));
#14230=CARTESIAN_POINT('',(11.6881451897504,333.257395605323,13.6889467097843));
#14231=CARTESIAN_POINT('Origin',(0.,10.75,0.));
#14232=CARTESIAN_POINT('Origin',(0.,10.75,0.));
#14233=CARTESIAN_POINT('',(9.4071264732029,10.7500000000001,15.3462038145323));
#14234=CARTESIAN_POINT('',(9.40712647320289,-5.75,15.3462038145323));
#14235=CARTESIAN_POINT('',(9.4071264732029,333.257395605323,15.3462038145323));
#14236=CARTESIAN_POINT('',(9.40282167159022,-5.74999999999998,15.3488418003533));
#14237=CARTESIAN_POINT('Origin',(0.,-5.75,0.));
#14238=CARTESIAN_POINT('',(9.40282167159023,10.7500000000001,15.3488418003533));
#14239=CARTESIAN_POINT('',(9.40282167159023,333.257395605323,15.3488418003533));
#14240=CARTESIAN_POINT('Origin',(0.,10.75,0.));
#14241=CARTESIAN_POINT('Origin',(0.,10.75,0.));
#14242=CARTESIAN_POINT('',(6.89063395196164,10.7500000000001,16.6288653774115));
#14243=CARTESIAN_POINT('',(6.89063395196164,-5.75,16.6288653774115));
#14244=CARTESIAN_POINT('',(6.89063395196164,333.257395605323,16.6288653774115));
#14245=CARTESIAN_POINT('',(6.88596947769954,-5.74999999999998,16.6307974659122));
#14246=CARTESIAN_POINT('Origin',(0.,-5.75,0.));
#14247=CARTESIAN_POINT('',(6.88596947769954,10.7500000000001,16.6307974659122));
#14248=CARTESIAN_POINT('',(6.88596947769954,333.257395605323,16.6307974659122));
#14249=CARTESIAN_POINT('Origin',(0.,10.75,0.));
#14250=CARTESIAN_POINT('Origin',(0.,10.75,0.));
#14251=CARTESIAN_POINT('',(4.20447115412013,10.7500000000001,17.5020690866586));
#14252=CARTESIAN_POINT('',(4.20447115412013,-5.75,17.5020690866586));
#14253=CARTESIAN_POINT('',(4.20447115412013,333.257395605323,17.5020690866586));
#14254=CARTESIAN_POINT('',(4.19956186204543,-5.74999999999998,17.5032477034079));
#14255=CARTESIAN_POINT('Origin',(0.,-5.75,0.));
#14256=CARTESIAN_POINT('',(4.19956186204542,10.7500000000001,17.5032477034079));
#14257=CARTESIAN_POINT('',(4.19956186204542,333.257395605323,17.5032477034079));
#14258=CARTESIAN_POINT('Origin',(0.,10.75,0.));
#14259=CARTESIAN_POINT('Origin',(0.,10.75,0.));
#14260=CARTESIAN_POINT('',(1.41478032262442,10.7500000000001,17.9443137689552));
#14261=CARTESIAN_POINT('',(1.41478032262442,-5.75,17.9443137689552));
#14262=CARTESIAN_POINT('',(1.41478032262442,333.257395605323,17.9443137689552));
#14263=CARTESIAN_POINT('',(1.409747095801,-5.74999999999998,17.944709892497));
#14264=CARTESIAN_POINT('Origin',(0.,-5.75,0.));
#14265=CARTESIAN_POINT('',(1.409747095801,10.7500000000001,17.944709892497));
#14266=CARTESIAN_POINT('',(1.409747095801,333.257395605323,17.944709892497));
#14267=CARTESIAN_POINT('Origin',(0.,10.75,0.));
#14268=CARTESIAN_POINT('Origin',(0.,10.75,0.));
#14269=CARTESIAN_POINT('',(-1.40974709580099,10.7500000000001,17.944709892497));
#14270=CARTESIAN_POINT('',(-1.40974709580099,-5.75,17.944709892497));
#14271=CARTESIAN_POINT('',(-1.40974709580099,333.257395605323,17.944709892497));
#14272=CARTESIAN_POINT('',(-1.41478032262415,-5.74999999999998,17.9443137689552));
#14273=CARTESIAN_POINT('Origin',(0.,-5.75,0.));
#14274=CARTESIAN_POINT('',(-1.41478032262415,10.7500000000001,17.9443137689552));
#14275=CARTESIAN_POINT('',(-1.41478032262415,333.257395605323,17.9443137689552));
#14276=CARTESIAN_POINT('Origin',(0.,10.75,0.));
#14277=CARTESIAN_POINT('Origin',(2.35100371814953E-15,333.257395605323,
18.9983764079945));
#14278=CARTESIAN_POINT('',(2.35100371814953E-15,-5.74999999999998,18.9983764079945));
#14279=CARTESIAN_POINT('',(2.35100371814953E-15,-5.74999999999998,18.9983764079945));
#14280=CARTESIAN_POINT('',(2.35100371814953E-15,10.7500000000001,18.9983764079945));
#14281=CARTESIAN_POINT('',(2.35100371814953E-15,333.257395605323,18.9983764079945));
#14282=CARTESIAN_POINT('',(9.1103600220179,10.75,12.1891541525139));
#14283=CARTESIAN_POINT('Origin',(2.35100371814953E-15,333.257395605323,
18.9983764079945));
#14284=CARTESIAN_POINT('',(2.35100371814953E-15,-5.74999999999998,18.9983764079945));
#14285=CARTESIAN_POINT('',(-9.11036002201789,10.75,12.1891541525139));
#14286=CARTESIAN_POINT('Origin',(2.97200085001758,333.257395605323,18.7644748684139));
#14287=CARTESIAN_POINT('',(2.97200085001758,-5.74999999999998,18.7644748684139));
#14288=CARTESIAN_POINT('',(2.97200085001758,-5.74999999999998,18.7644748684139));
#14289=CARTESIAN_POINT('',(2.97200085001758,10.7500000000001,18.7644748684139));
#14290=CARTESIAN_POINT('',(2.97200085001758,333.257395605323,18.7644748684139));
#14291=CARTESIAN_POINT('',(10.9050001815126,10.75,10.6139111417865));
#14292=CARTESIAN_POINT('Origin',(2.97200085001758,333.257395605323,18.7644748684139));
#14293=CARTESIAN_POINT('',(2.97200085001758,-5.74999999999998,18.7644748684139));
#14294=CARTESIAN_POINT('',(-7.09139256322972,10.75,13.4642597345231));
#14295=CARTESIAN_POINT('Origin',(5.8708211756024,333.257395605323,18.0685296818513));
#14296=CARTESIAN_POINT('',(5.8708211756024,-5.74999999999998,18.0685296818513));
#14297=CARTESIAN_POINT('',(5.8708211756024,-5.74999999999998,18.0685296818513));
#14298=CARTESIAN_POINT('',(5.8708211756024,10.7500000000001,18.0685296818513));
#14299=CARTESIAN_POINT('',(5.8708211756024,333.257395605323,18.0685296818513));
#14300=CARTESIAN_POINT('',(12.4311230449177,10.75,8.77731841319679));
#14301=CARTESIAN_POINT('Origin',(5.8708211756024,333.257395605323,18.0685296818513));
#14302=CARTESIAN_POINT('',(5.8708211756024,-5.74999999999998,18.0685296818513));
#14303=CARTESIAN_POINT('',(-4.89781148455222,10.75,14.4078305565521));
#14304=CARTESIAN_POINT('Origin',(8.62508239970547,333.257395605323,16.9276773285095));
#14305=CARTESIAN_POINT('',(8.62508239970547,-5.74999999999998,16.9276773285095));
#14306=CARTESIAN_POINT('',(8.62508239970547,-5.74999999999998,16.9276773285095));
#14307=CARTESIAN_POINT('',(8.62508239970547,10.7500000000001,16.9276773285095));
#14308=CARTESIAN_POINT('',(8.62508239970547,333.257395605323,16.9276773285095));
#14309=CARTESIAN_POINT('',(13.651150402425,10.75,6.72459897502448));
#14310=CARTESIAN_POINT('Origin',(8.62508239970547,333.257395605323,16.9276773285095));
#14311=CARTESIAN_POINT('',(8.62508239970547,-5.74999999999998,16.9276773285095));
#14312=CARTESIAN_POINT('',(-2.58363003222066,10.75,14.9966327734307));
#14313=CARTESIAN_POINT('Origin',(11.1669654701205,333.257395605323,15.3700093795996));
#14314=CARTESIAN_POINT('',(11.1669654701205,-5.74999999999998,15.3700093795996));
#14315=CARTESIAN_POINT('',(11.1669654701205,-5.74999999999998,15.3700093795996));
#14316=CARTESIAN_POINT('',(11.1669654701205,10.7500000000001,15.3700093795996));
#14317=CARTESIAN_POINT('',(11.1669654701205,333.257395605323,15.3700093795996));
#14318=CARTESIAN_POINT('',(14.5350411314538,10.75,4.50629759242261));
#14319=CARTESIAN_POINT('Origin',(11.1669654701205,333.257395605323,15.3700093795996));
#14320=CARTESIAN_POINT('',(11.1669654701205,-5.74999999999998,15.3700093795996));
#14321=CARTESIAN_POINT('',(-0.205831033919359,10.75,15.2161681204567));
#14322=CARTESIAN_POINT('Origin',(13.4338807896275,333.257395605323,13.4338807896274));
#14323=CARTESIAN_POINT('',(13.4338807896275,-5.74999999999998,13.4338807896274));
#14324=CARTESIAN_POINT('',(13.4338807896275,-5.74999999999998,13.4338807896274));
#14325=CARTESIAN_POINT('',(13.4338807896275,10.7500000000001,13.4338807896274));
#14326=CARTESIAN_POINT('',(13.4338807896275,333.257395605323,13.4338807896274));
#14327=CARTESIAN_POINT('',(15.0610309087904,10.75,2.17703620755101));
#14328=CARTESIAN_POINT('Origin',(13.4338807896275,333.257395605323,13.4338807896274));
#14329=CARTESIAN_POINT('',(13.4338807896275,-5.74999999999998,13.4338807896274));
#14330=CARTESIAN_POINT('',(2.17703620755108,10.75,15.0610309087904));
#14331=CARTESIAN_POINT('Origin',(15.3700093795997,333.257395605323,11.1669654701204));
#14332=CARTESIAN_POINT('',(15.3700093795997,-5.74999999999998,11.1669654701204));
#14333=CARTESIAN_POINT('',(15.3700093795997,-5.74999999999998,11.1669654701204));
#14334=CARTESIAN_POINT('',(15.3700093795997,10.7500000000001,11.1669654701204));
#14335=CARTESIAN_POINT('',(15.3700093795997,333.257395605323,11.1669654701204));
#14336=CARTESIAN_POINT('',(15.2161681204567,10.75,-0.205831033919424));
#14337=CARTESIAN_POINT('Origin',(15.3700093795997,333.257395605323,11.1669654701204));
#14338=CARTESIAN_POINT('',(15.3700093795997,-5.74999999999998,11.1669654701204));
#14339=CARTESIAN_POINT('',(4.50629759242267,10.75,14.5350411314538));
#14340=CARTESIAN_POINT('Origin',(16.9276773285095,333.257395605323,8.62508239970541));
#14341=CARTESIAN_POINT('',(16.9276773285095,-5.74999999999998,8.62508239970541));
#14342=CARTESIAN_POINT('',(16.9276773285095,-5.74999999999998,8.62508239970541));
#14343=CARTESIAN_POINT('',(16.9276773285095,10.7500000000001,8.62508239970541));
#14344=CARTESIAN_POINT('',(16.9276773285095,333.257395605323,8.62508239970541));
#14345=CARTESIAN_POINT('',(14.9966327734307,10.75,-2.58363003222073));
#14346=CARTESIAN_POINT('Origin',(16.9276773285095,333.257395605323,8.62508239970541));
#14347=CARTESIAN_POINT('',(16.9276773285095,-5.74999999999998,8.62508239970541));
#14348=CARTESIAN_POINT('',(6.72459897502454,10.75,13.651150402425));
#14349=CARTESIAN_POINT('Origin',(18.0685296818513,333.257395605323,5.87082117560233));
#14350=CARTESIAN_POINT('',(18.0685296818513,-5.74999999999998,5.87082117560233));
#14351=CARTESIAN_POINT('',(18.0685296818513,-5.74999999999998,5.87082117560233));
#14352=CARTESIAN_POINT('',(18.0685296818513,10.7500000000001,5.87082117560233));
#14353=CARTESIAN_POINT('',(18.0685296818513,333.257395605323,5.87082117560233));
#14354=CARTESIAN_POINT('',(14.4078305565521,10.75,-4.89781148455228));
#14355=CARTESIAN_POINT('Origin',(18.0685296818513,333.257395605323,5.87082117560233));
#14356=CARTESIAN_POINT('',(18.0685296818513,-5.74999999999998,5.87082117560233));
#14357=CARTESIAN_POINT('',(8.77731841319684,10.75,12.4311230449177));
#14358=CARTESIAN_POINT('Origin',(18.7644748684139,333.257395605323,2.9720008500175));
#14359=CARTESIAN_POINT('',(18.7644748684139,-5.74999999999998,2.9720008500175));
#14360=CARTESIAN_POINT('',(18.7644748684139,-5.74999999999998,2.9720008500175));
#14361=CARTESIAN_POINT('',(18.7644748684139,10.7500000000001,2.9720008500175));
#14362=CARTESIAN_POINT('',(18.7644748684139,333.257395605323,2.9720008500175));
#14363=CARTESIAN_POINT('',(13.464259734523,10.75,-7.09139256322977));
#14364=CARTESIAN_POINT('Origin',(18.7644748684139,333.257395605323,2.9720008500175));
#14365=CARTESIAN_POINT('',(18.7644748684139,-5.74999999999998,2.9720008500175));
#14366=CARTESIAN_POINT('',(10.6139111417865,10.75,10.9050001815125));
#14367=CARTESIAN_POINT('Origin',(18.9983764079945,333.257395605323,-6.86834804149801E-14));
#14368=CARTESIAN_POINT('',(18.9983764079945,-5.74999999999998,-6.86834804149801E-14));
#14369=CARTESIAN_POINT('',(18.9983764079945,-5.74999999999998,-6.86834804149801E-14));
#14370=CARTESIAN_POINT('',(18.9983764079945,10.7500000000001,-6.86834804149801E-14));
#14371=CARTESIAN_POINT('',(18.9983764079945,333.257395605323,-6.86834804149801E-14));
#14372=CARTESIAN_POINT('',(12.1891541525138,10.75,-9.11036002201794));
#14373=CARTESIAN_POINT('Origin',(18.9983764079945,333.257395605323,-6.86834804149801E-14));
#14374=CARTESIAN_POINT('',(18.9983764079945,-5.74999999999998,-6.86834804149801E-14));
#14375=CARTESIAN_POINT('',(12.1891541525139,10.75,9.11036002201785));
#14376=CARTESIAN_POINT('Origin',(18.7644748684139,333.257395605323,-2.97200085001764));
#14377=CARTESIAN_POINT('',(18.7644748684139,-5.74999999999998,-2.97200085001764));
#14378=CARTESIAN_POINT('',(18.7644748684139,-5.74999999999998,-2.97200085001764));
#14379=CARTESIAN_POINT('',(18.7644748684139,10.7500000000001,-2.97200085001764));
#14380=CARTESIAN_POINT('',(18.7644748684139,333.257395605323,-2.97200085001764));
#14381=CARTESIAN_POINT('',(10.6139111417864,10.75,-10.9050001815126));
#14382=CARTESIAN_POINT('Origin',(18.7644748684139,333.257395605323,-2.97200085001764));
#14383=CARTESIAN_POINT('',(18.7644748684139,-5.74999999999998,-2.97200085001764));
#14384=CARTESIAN_POINT('',(13.4642597345231,10.75,7.09139256322967));
#14385=CARTESIAN_POINT('Origin',(18.0685296818513,333.257395605323,-5.87082117560246));
#14386=CARTESIAN_POINT('',(18.0685296818513,-5.74999999999998,-5.87082117560246));
#14387=CARTESIAN_POINT('',(18.0685296818513,-5.74999999999998,-5.87082117560246));
#14388=CARTESIAN_POINT('',(18.0685296818513,10.7500000000001,-5.87082117560246));
#14389=CARTESIAN_POINT('',(18.0685296818513,333.257395605323,-5.87082117560246));
#14390=CARTESIAN_POINT('',(8.77731841319674,10.75,-12.4311230449178));
#14391=CARTESIAN_POINT('Origin',(18.0685296818513,333.257395605323,-5.87082117560246));
#14392=CARTESIAN_POINT('',(18.0685296818513,-5.74999999999998,-5.87082117560246));
#14393=CARTESIAN_POINT('',(14.4078305565521,10.75,4.89781148455217));
#14394=CARTESIAN_POINT('Origin',(16.9276773285095,333.257395605323,-8.62508239970554));
#14395=CARTESIAN_POINT('',(16.9276773285095,-5.74999999999998,-8.62508239970554));
#14396=CARTESIAN_POINT('',(16.9276773285095,-5.74999999999998,-8.62508239970554));
#14397=CARTESIAN_POINT('',(16.9276773285095,10.7500000000001,-8.62508239970554));
#14398=CARTESIAN_POINT('',(16.9276773285095,333.257395605323,-8.62508239970554));
#14399=CARTESIAN_POINT('',(6.72459897502443,10.75,-13.651150402425));
#14400=CARTESIAN_POINT('Origin',(16.9276773285095,333.257395605323,-8.62508239970554));
#14401=CARTESIAN_POINT('',(16.9276773285095,-5.74999999999998,-8.62508239970554));
#14402=CARTESIAN_POINT('',(14.9966327734307,10.75,2.58363003222061));
#14403=CARTESIAN_POINT('Origin',(15.3700093795996,333.257395605323,-11.1669654701205));
#14404=CARTESIAN_POINT('',(15.3700093795996,-5.74999999999998,-11.1669654701205));
#14405=CARTESIAN_POINT('',(15.3700093795996,-5.74999999999998,-11.1669654701205));
#14406=CARTESIAN_POINT('',(15.3700093795996,10.7500000000001,-11.1669654701205));
#14407=CARTESIAN_POINT('',(15.3700093795996,333.257395605323,-11.1669654701205));
#14408=CARTESIAN_POINT('',(4.50629759242255,10.75,-14.5350411314538));
#14409=CARTESIAN_POINT('Origin',(15.3700093795996,333.257395605323,-11.1669654701205));
#14410=CARTESIAN_POINT('',(15.3700093795996,-5.74999999999998,-11.1669654701205));
#14411=CARTESIAN_POINT('',(15.2161681204567,10.75,0.205831033919306));
#14412=CARTESIAN_POINT('Origin',(13.4338807896274,333.257395605323,-13.4338807896275));
#14413=CARTESIAN_POINT('',(13.4338807896274,-5.74999999999998,-13.4338807896275));
#14414=CARTESIAN_POINT('',(13.4338807896274,-5.74999999999998,-13.4338807896275));
#14415=CARTESIAN_POINT('',(13.4338807896274,10.7500000000001,-13.4338807896275));
#14416=CARTESIAN_POINT('',(13.4338807896274,333.257395605323,-13.4338807896275));
#14417=CARTESIAN_POINT('',(2.17703620755096,10.75,-15.0610309087904));
#14418=CARTESIAN_POINT('Origin',(13.4338807896274,333.257395605323,-13.4338807896275));
#14419=CARTESIAN_POINT('',(13.4338807896274,-5.74999999999998,-13.4338807896275));
#14420=CARTESIAN_POINT('',(15.0610309087904,10.75,-2.17703620755113));
#14421=CARTESIAN_POINT('Origin',(11.1669654701203,333.257395605323,-15.3700093795997));
#14422=CARTESIAN_POINT('',(11.1669654701203,-5.74999999999998,-15.3700093795997));
#14423=CARTESIAN_POINT('',(11.1669654701203,-5.74999999999998,-15.3700093795997));
#14424=CARTESIAN_POINT('',(11.1669654701203,10.7500000000001,-15.3700093795997));
#14425=CARTESIAN_POINT('',(11.1669654701203,333.257395605323,-15.3700093795997));
#14426=CARTESIAN_POINT('',(-0.205831033919478,10.75,-15.2161681204567));
#14427=CARTESIAN_POINT('Origin',(11.1669654701203,333.257395605323,-15.3700093795997));
#14428=CARTESIAN_POINT('',(11.1669654701203,-5.74999999999998,-15.3700093795997));
#14429=CARTESIAN_POINT('',(14.5350411314538,10.75,-4.50629759242272));
#14430=CARTESIAN_POINT('Origin',(8.62508239970535,333.257395605323,-16.9276773285096));
#14431=CARTESIAN_POINT('',(8.62508239970535,-5.74999999999998,-16.9276773285096));
#14432=CARTESIAN_POINT('',(8.62508239970535,-5.74999999999998,-16.9276773285096));
#14433=CARTESIAN_POINT('',(8.62508239970535,10.7500000000001,-16.9276773285096));
#14434=CARTESIAN_POINT('',(8.62508239970535,333.257395605323,-16.9276773285096));
#14435=CARTESIAN_POINT('',(-2.58363003222078,10.75,-14.9966327734307));
#14436=CARTESIAN_POINT('Origin',(8.62508239970535,333.257395605323,-16.9276773285096));
#14437=CARTESIAN_POINT('',(8.62508239970535,-5.74999999999998,-16.9276773285096));
#14438=CARTESIAN_POINT('',(13.6511504024249,10.75,-6.72459897502459));
#14439=CARTESIAN_POINT('Origin',(5.87082117560226,333.257395605323,-18.0685296818514));
#14440=CARTESIAN_POINT('',(5.87082117560226,-5.74999999999998,-18.0685296818514));
#14441=CARTESIAN_POINT('',(5.87082117560226,-5.74999999999998,-18.0685296818514));
#14442=CARTESIAN_POINT('',(5.87082117560226,10.7500000000001,-18.0685296818514));
#14443=CARTESIAN_POINT('',(5.87082117560226,333.257395605323,-18.0685296818514));
#14444=CARTESIAN_POINT('',(-4.89781148455233,10.75,-14.4078305565521));
#14445=CARTESIAN_POINT('Origin',(5.87082117560226,333.257395605323,-18.0685296818514));
#14446=CARTESIAN_POINT('',(5.87082117560226,-5.74999999999998,-18.0685296818514));
#14447=CARTESIAN_POINT('',(12.4311230449177,10.75,-8.77731841319689));
#14448=CARTESIAN_POINT('Origin',(2.97200085001744,333.257395605323,-18.764474868414));
#14449=CARTESIAN_POINT('',(2.97200085001744,-5.74999999999998,-18.764474868414));
#14450=CARTESIAN_POINT('',(2.97200085001744,-5.74999999999998,-18.764474868414));
#14451=CARTESIAN_POINT('',(2.97200085001744,10.7500000000001,-18.764474868414));
#14452=CARTESIAN_POINT('',(2.97200085001744,333.257395605323,-18.764474868414));
#14453=CARTESIAN_POINT('',(-7.09139256322982,10.75,-13.464259734523));
#14454=CARTESIAN_POINT('Origin',(2.97200085001744,333.257395605323,-18.764474868414));
#14455=CARTESIAN_POINT('',(2.97200085001744,-5.74999999999998,-18.764474868414));
#14456=CARTESIAN_POINT('',(10.9050001815125,10.75,-10.6139111417866));
#14457=CARTESIAN_POINT('Origin',(-2.35100371814953E-15,333.257395605323,
-18.9983764079945));
#14458=CARTESIAN_POINT('',(-2.35100371814953E-15,-5.74999999999998,-18.9983764079945));
#14459=CARTESIAN_POINT('',(-2.35100371814953E-15,-5.74999999999998,-18.9983764079945));
#14460=CARTESIAN_POINT('',(-2.35100371814953E-15,10.7500000000001,-18.9983764079945));
#14461=CARTESIAN_POINT('',(-2.35100371814953E-15,333.257395605323,-18.9983764079945));
#14462=CARTESIAN_POINT('',(-9.1103600220179,10.75,-12.1891541525139));
#14463=CARTESIAN_POINT('Origin',(-2.35100371814953E-15,333.257395605323,
-18.9983764079945));
#14464=CARTESIAN_POINT('',(-2.35100371814953E-15,-5.74999999999998,-18.9983764079945));
#14465=CARTESIAN_POINT('',(9.11036002201789,10.75,-12.1891541525139));
#14466=CARTESIAN_POINT('Origin',(-2.97200085001771,333.257395605323,-18.7644748684139));
#14467=CARTESIAN_POINT('',(-2.97200085001771,-5.74999999999998,-18.7644748684139));
#14468=CARTESIAN_POINT('',(-2.97200085001771,-5.74999999999998,-18.7644748684139));
#14469=CARTESIAN_POINT('',(-2.97200085001771,10.7500000000001,-18.7644748684139));
#14470=CARTESIAN_POINT('',(-2.97200085001771,333.257395605323,-18.7644748684139));
#14471=CARTESIAN_POINT('',(-10.9050001815126,10.75,-10.6139111417864));
#14472=CARTESIAN_POINT('Origin',(-2.97200085001771,333.257395605323,-18.7644748684139));
#14473=CARTESIAN_POINT('',(-2.97200085001771,-5.74999999999998,-18.7644748684139));
#14474=CARTESIAN_POINT('',(7.09139256322962,10.75,-13.4642597345231));
#14475=CARTESIAN_POINT('Origin',(-5.87082117560253,333.257395605323,-18.0685296818513));
#14476=CARTESIAN_POINT('',(-5.87082117560253,-5.74999999999998,-18.0685296818513));
#14477=CARTESIAN_POINT('',(-5.87082117560253,-5.74999999999998,-18.0685296818513));
#14478=CARTESIAN_POINT('',(-5.87082117560253,10.7500000000001,-18.0685296818513));
#14479=CARTESIAN_POINT('',(-5.87082117560253,333.257395605323,-18.0685296818513));
#14480=CARTESIAN_POINT('',(-12.4311230449178,10.75,-8.7773184131967));
#14481=CARTESIAN_POINT('Origin',(-5.87082117560253,333.257395605323,-18.0685296818513));
#14482=CARTESIAN_POINT('',(-5.87082117560253,-5.74999999999998,-18.0685296818513));
#14483=CARTESIAN_POINT('',(4.89781148455211,10.75,-14.4078305565521));
#14484=CARTESIAN_POINT('Origin',(-8.6250823997056,333.257395605323,-16.9276773285094));
#14485=CARTESIAN_POINT('',(-8.6250823997056,-5.74999999999998,-16.9276773285094));
#14486=CARTESIAN_POINT('',(-8.6250823997056,-5.74999999999998,-16.9276773285094));
#14487=CARTESIAN_POINT('',(-8.6250823997056,10.7500000000001,-16.9276773285094));
#14488=CARTESIAN_POINT('',(-8.6250823997056,333.257395605323,-16.9276773285094));
#14489=CARTESIAN_POINT('',(-13.651150402425,10.75,-6.72459897502439));
#14490=CARTESIAN_POINT('Origin',(-8.6250823997056,333.257395605323,-16.9276773285094));
#14491=CARTESIAN_POINT('',(-8.6250823997056,-5.74999999999998,-16.9276773285094));
#14492=CARTESIAN_POINT('',(2.58363003222055,10.75,-14.9966327734307));
#14493=CARTESIAN_POINT('Origin',(-11.1669654701206,333.257395605323,-15.3700093795995));
#14494=CARTESIAN_POINT('',(-11.1669654701206,-5.74999999999998,-15.3700093795995));
#14495=CARTESIAN_POINT('',(-11.1669654701206,-5.74999999999998,-15.3700093795995));
#14496=CARTESIAN_POINT('',(-11.1669654701206,10.7500000000001,-15.3700093795995));
#14497=CARTESIAN_POINT('',(-11.1669654701206,333.257395605323,-15.3700093795995));
#14498=CARTESIAN_POINT('',(-14.5350411314539,10.75,-4.5062975924225));
#14499=CARTESIAN_POINT('Origin',(-11.1669654701206,333.257395605323,-15.3700093795995));
#14500=CARTESIAN_POINT('',(-11.1669654701206,-5.74999999999998,-15.3700093795995));
#14501=CARTESIAN_POINT('',(0.205831033919245,10.75,-15.2161681204567));
#14502=CARTESIAN_POINT('Origin',(-13.4338807896276,333.257395605323,-13.4338807896273));
#14503=CARTESIAN_POINT('',(-13.4338807896276,-5.74999999999998,-13.4338807896273));
#14504=CARTESIAN_POINT('',(-13.4338807896276,-5.74999999999998,-13.4338807896273));
#14505=CARTESIAN_POINT('',(-13.4338807896276,10.7500000000001,-13.4338807896273));
#14506=CARTESIAN_POINT('',(-13.4338807896276,333.257395605323,-13.4338807896273));
#14507=CARTESIAN_POINT('',(-15.0610309087904,10.75,-2.17703620755091));
#14508=CARTESIAN_POINT('Origin',(-13.4338807896276,333.257395605323,-13.4338807896273));
#14509=CARTESIAN_POINT('',(-13.4338807896276,-5.74999999999998,-13.4338807896273));
#14510=CARTESIAN_POINT('',(-2.17703620755118,10.75,-15.0610309087904));
#14511=CARTESIAN_POINT('Origin',(-15.3700093795998,333.257395605323,-11.1669654701203));
#14512=CARTESIAN_POINT('',(-15.3700093795998,-5.74999999999998,-11.1669654701203));
#14513=CARTESIAN_POINT('',(-15.3700093795998,-5.74999999999998,-11.1669654701203));
#14514=CARTESIAN_POINT('',(-15.3700093795998,10.7500000000001,-11.1669654701203));
#14515=CARTESIAN_POINT('',(-15.3700093795998,333.257395605323,-11.1669654701203));
#14516=CARTESIAN_POINT('',(-15.2161681204567,10.75,0.205831033919538));
#14517=CARTESIAN_POINT('Origin',(-15.3700093795998,333.257395605323,-11.1669654701203));
#14518=CARTESIAN_POINT('',(-15.3700093795998,-5.74999999999998,-11.1669654701203));
#14519=CARTESIAN_POINT('',(-4.50629759242278,10.75,-14.5350411314538));
#14520=CARTESIAN_POINT('Origin',(-16.9276773285096,333.257395605323,-8.62508239970529));
#14521=CARTESIAN_POINT('',(-16.9276773285096,-5.74999999999998,-8.62508239970529));
#14522=CARTESIAN_POINT('',(-16.9276773285096,-5.74999999999998,-8.62508239970529));
#14523=CARTESIAN_POINT('',(-16.9276773285096,10.7500000000001,-8.62508239970529));
#14524=CARTESIAN_POINT('',(-16.9276773285096,333.257395605323,-8.62508239970529));
#14525=CARTESIAN_POINT('',(-14.9966327734307,10.75,2.58363003222083));
#14526=CARTESIAN_POINT('Origin',(-16.9276773285096,333.257395605323,-8.62508239970529));
#14527=CARTESIAN_POINT('',(-16.9276773285096,-5.74999999999998,-8.62508239970529));
#14528=CARTESIAN_POINT('',(-6.72459897502464,10.75,-13.6511504024249));
#14529=CARTESIAN_POINT('Origin',(-18.0685296818514,333.257395605323,-5.8708211756022));
#14530=CARTESIAN_POINT('',(-18.0685296818514,-5.74999999999998,-5.8708211756022));
#14531=CARTESIAN_POINT('',(-18.0685296818514,-5.74999999999998,-5.8708211756022));
#14532=CARTESIAN_POINT('',(-18.0685296818514,10.7500000000001,-5.8708211756022));
#14533=CARTESIAN_POINT('',(-18.0685296818514,333.257395605323,-5.8708211756022));
#14534=CARTESIAN_POINT('',(-14.407830556552,10.75,4.89781148455238));
#14535=CARTESIAN_POINT('Origin',(-18.0685296818514,333.257395605323,-5.8708211756022));
#14536=CARTESIAN_POINT('',(-18.0685296818514,-5.74999999999998,-5.8708211756022));
#14537=CARTESIAN_POINT('',(-8.77731841319692,10.75,-12.4311230449176));
#14538=CARTESIAN_POINT('Origin',(-18.764474868414,333.257395605323,-2.97200085001737));
#14539=CARTESIAN_POINT('',(-18.764474868414,-5.74999999999998,-2.97200085001737));
#14540=CARTESIAN_POINT('',(-18.764474868414,-5.74999999999998,-2.97200085001737));
#14541=CARTESIAN_POINT('',(-18.764474868414,10.7500000000001,-2.97200085001737));
#14542=CARTESIAN_POINT('',(-18.764474868414,333.257395605323,-2.97200085001737));
#14543=CARTESIAN_POINT('',(-13.464259734523,10.75,7.09139256322987));
#14544=CARTESIAN_POINT('Origin',(-18.764474868414,333.257395605323,-2.97200085001737));
#14545=CARTESIAN_POINT('',(-18.764474868414,-5.74999999999998,-2.97200085001737));
#14546=CARTESIAN_POINT('',(-10.6139111417866,10.75,-10.9050001815124));
#14547=CARTESIAN_POINT('Origin',(-18.9983764079945,333.257395605323,2.01348433808641E-13));
#14548=CARTESIAN_POINT('',(-18.9983764079945,-5.74999999999998,2.01348433808641E-13));
#14549=CARTESIAN_POINT('',(-18.9983764079945,-5.74999999999998,2.01348433808641E-13));
#14550=CARTESIAN_POINT('',(-18.9983764079945,10.7500000000001,2.01348433808641E-13));
#14551=CARTESIAN_POINT('',(-18.9983764079945,333.257395605323,2.01348433808641E-13));
#14552=CARTESIAN_POINT('',(-12.1891541525138,10.75,9.11036002201803));
#14553=CARTESIAN_POINT('Origin',(-18.9983764079945,333.257395605323,2.01348433808641E-13));
#14554=CARTESIAN_POINT('',(-18.9983764079945,-5.74999999999998,2.01348433808641E-13));
#14555=CARTESIAN_POINT('',(-12.189154152514,10.75,-9.11036002201777));
#14556=CARTESIAN_POINT('Origin',(-18.7644748684139,333.257395605323,2.97200085001778));
#14557=CARTESIAN_POINT('',(-18.7644748684139,-5.74999999999998,2.97200085001778));
#14558=CARTESIAN_POINT('',(-18.7644748684139,-5.74999999999998,2.97200085001778));
#14559=CARTESIAN_POINT('',(-18.7644748684139,10.7500000000001,2.97200085001778));
#14560=CARTESIAN_POINT('',(-18.7644748684139,333.257395605323,2.97200085001778));
#14561=CARTESIAN_POINT('',(-10.6139111417864,10.75,10.9050001815127));
#14562=CARTESIAN_POINT('Origin',(-18.7644748684139,333.257395605323,2.97200085001778));
#14563=CARTESIAN_POINT('',(-18.7644748684139,-5.74999999999998,2.97200085001778));
#14564=CARTESIAN_POINT('',(-13.4642597345231,10.75,-7.09139256322957));
#14565=CARTESIAN_POINT('Origin',(-18.0685296818512,333.257395605323,5.87082117560259));
#14566=CARTESIAN_POINT('',(-18.0685296818512,-5.74999999999998,5.87082117560259));
#14567=CARTESIAN_POINT('',(-18.0685296818512,-5.74999999999998,5.87082117560259));
#14568=CARTESIAN_POINT('',(-18.0685296818512,10.7500000000001,5.87082117560259));
#14569=CARTESIAN_POINT('',(-18.0685296818512,333.257395605323,5.87082117560259));
#14570=CARTESIAN_POINT('',(-8.77731841319665,10.75,12.4311230449178));
#14571=CARTESIAN_POINT('Origin',(-18.0685296818512,333.257395605323,5.87082117560259));
#14572=CARTESIAN_POINT('',(-18.0685296818512,-5.74999999999998,5.87082117560259));
#14573=CARTESIAN_POINT('',(-14.4078305565522,10.75,-4.89781148455206));
#14574=CARTESIAN_POINT('Origin',(-16.9276773285094,333.257395605323,8.62508239970565));
#14575=CARTESIAN_POINT('',(-16.9276773285094,-5.74999999999998,8.62508239970565));
#14576=CARTESIAN_POINT('',(-16.9276773285094,-5.74999999999998,8.62508239970565));
#14577=CARTESIAN_POINT('',(-16.9276773285094,10.7500000000001,8.62508239970565));
#14578=CARTESIAN_POINT('',(-16.9276773285094,333.257395605323,8.62508239970565));
#14579=CARTESIAN_POINT('',(-6.72459897502434,10.75,13.6511504024251));
#14580=CARTESIAN_POINT('Origin',(-16.9276773285094,333.257395605323,8.62508239970565));
#14581=CARTESIAN_POINT('',(-16.9276773285094,-5.74999999999998,8.62508239970565));
#14582=CARTESIAN_POINT('',(-14.9966327734307,10.75,-2.58363003222051));
#14583=CARTESIAN_POINT('Origin',(-15.3700093795995,333.257395605323,11.1669654701206));
#14584=CARTESIAN_POINT('',(-15.3700093795995,-5.74999999999998,11.1669654701206));
#14585=CARTESIAN_POINT('',(-15.3700093795995,-5.74999999999998,11.1669654701206));
#14586=CARTESIAN_POINT('',(-15.3700093795995,10.7500000000001,11.1669654701206));
#14587=CARTESIAN_POINT('',(-15.3700093795995,333.257395605323,11.1669654701206));
#14588=CARTESIAN_POINT('',(-4.50629759242245,10.75,14.5350411314539));
#14589=CARTESIAN_POINT('Origin',(-15.3700093795995,333.257395605323,11.1669654701206));
#14590=CARTESIAN_POINT('',(-15.3700093795995,-5.74999999999998,11.1669654701206));
#14591=CARTESIAN_POINT('',(-15.2161681204567,10.75,-0.205831033919193));
#14592=CARTESIAN_POINT('Origin',(-13.4338807896273,333.257395605323,13.4338807896276));
#14593=CARTESIAN_POINT('',(-13.4338807896273,-5.74999999999998,13.4338807896276));
#14594=CARTESIAN_POINT('',(-13.4338807896273,-5.74999999999998,13.4338807896276));
#14595=CARTESIAN_POINT('',(-13.4338807896273,10.7500000000001,13.4338807896276));
#14596=CARTESIAN_POINT('',(-13.4338807896273,333.257395605323,13.4338807896276));
#14597=CARTESIAN_POINT('',(-2.17703620755086,10.75,15.0610309087904));
#14598=CARTESIAN_POINT('Origin',(-13.4338807896273,333.257395605323,13.4338807896276));
#14599=CARTESIAN_POINT('',(-13.4338807896273,-5.74999999999998,13.4338807896276));
#14600=CARTESIAN_POINT('',(-15.0610309087904,10.75,2.17703620755124));
#14601=CARTESIAN_POINT('Origin',(-11.1669654701202,333.257395605323,15.3700093795998));
#14602=CARTESIAN_POINT('',(-11.1669654701202,-5.74999999999998,15.3700093795998));
#14603=CARTESIAN_POINT('',(-11.1669654701202,-5.74999999999998,15.3700093795998));
#14604=CARTESIAN_POINT('',(-11.1669654701202,10.7500000000001,15.3700093795998));
#14605=CARTESIAN_POINT('',(-11.1669654701202,333.257395605323,15.3700093795998));
#14606=CARTESIAN_POINT('',(0.205831033919592,10.75,15.2161681204567));
#14607=CARTESIAN_POINT('Origin',(-11.1669654701202,333.257395605323,15.3700093795998));
#14608=CARTESIAN_POINT('',(-11.1669654701202,-5.74999999999998,15.3700093795998));
#14609=CARTESIAN_POINT('',(-14.5350411314538,10.75,4.50629759242283));
#14610=CARTESIAN_POINT('Origin',(-8.62508239970523,333.257395605323,16.9276773285096));
#14611=CARTESIAN_POINT('',(-8.62508239970523,-5.74999999999998,16.9276773285096));
#14612=CARTESIAN_POINT('',(-8.62508239970523,-5.74999999999998,16.9276773285096));
#14613=CARTESIAN_POINT('',(-8.62508239970523,10.7500000000001,16.9276773285096));
#14614=CARTESIAN_POINT('',(-8.62508239970523,333.257395605323,16.9276773285096));
#14615=CARTESIAN_POINT('',(2.58363003222089,10.75,14.9966327734307));
#14616=CARTESIAN_POINT('Origin',(-8.62508239970523,333.257395605323,16.9276773285096));
#14617=CARTESIAN_POINT('',(-8.62508239970523,-5.74999999999998,16.9276773285096));
#14618=CARTESIAN_POINT('',(-13.6511504024249,10.75,6.72459897502469));
#14619=CARTESIAN_POINT('Origin',(-5.87082117560214,333.257395605323,18.0685296818514));
#14620=CARTESIAN_POINT('',(-5.87082117560214,-5.74999999999998,18.0685296818514));
#14621=CARTESIAN_POINT('',(-5.87082117560214,-5.74999999999998,18.0685296818514));
#14622=CARTESIAN_POINT('',(-5.87082117560214,10.7500000000001,18.0685296818514));
#14623=CARTESIAN_POINT('',(-5.87082117560214,333.257395605323,18.0685296818514));
#14624=CARTESIAN_POINT('',(4.89781148455243,10.75,14.407830556552));
#14625=CARTESIAN_POINT('Origin',(-5.87082117560214,333.257395605323,18.0685296818514));
#14626=CARTESIAN_POINT('',(-5.87082117560214,-5.74999999999998,18.0685296818514));
#14627=CARTESIAN_POINT('',(-12.4311230449176,10.75,8.77731841319697));
#14628=CARTESIAN_POINT('Origin',(-2.9720008500173,333.257395605323,18.764474868414));
#14629=CARTESIAN_POINT('',(-2.9720008500173,-5.74999999999998,18.764474868414));
#14630=CARTESIAN_POINT('',(-2.9720008500173,-5.74999999999998,18.764474868414));
#14631=CARTESIAN_POINT('',(-2.9720008500173,10.7500000000001,18.764474868414));
#14632=CARTESIAN_POINT('',(-2.9720008500173,333.257395605323,18.764474868414));
#14633=CARTESIAN_POINT('',(7.09139256322992,10.75,13.4642597345229));
#14634=CARTESIAN_POINT('Origin',(-2.9720008500173,333.257395605323,18.764474868414));
#14635=CARTESIAN_POINT('',(-2.9720008500173,-5.74999999999998,18.764474868414));
#14636=CARTESIAN_POINT('',(-10.9050001815124,10.75,10.6139111417866));
#14637=CARTESIAN_POINT('Origin',(0.,10.75,0.));
#14638=CARTESIAN_POINT('',(-19.1556296640195,9.75000000013554,-16.0643184011738));
#14639=CARTESIAN_POINT('',(-19.1556295034202,-9.75000000012816,-16.0643182664888));
#14640=CARTESIAN_POINT('Ctrl Pts',(-19.1556296640195,9.75000000013554,-16.0643184011738));
#14641=CARTESIAN_POINT('Ctrl Pts',(-19.2208712137408,8.88364083244263,-15.986541870064));
#14642=CARTESIAN_POINT('Ctrl Pts',(-19.277148698093,8.01647570568422,-15.9184997691583));
#14643=CARTESIAN_POINT('Ctrl Pts',(-19.3246365744442,7.14847237162856,-15.8606239542862));
#14644=CARTESIAN_POINT('Ctrl Pts',(-19.3555503720308,6.58341700518073,-15.8229477858916));
#14645=CARTESIAN_POINT('Ctrl Pts',(-19.382739481617,6.01800679455978,-15.7895788865733));
#14646=CARTESIAN_POINT('Ctrl Pts',(-19.4062538058647,5.45223695733227,-15.760625407086));
#14647=CARTESIAN_POINT('Ctrl Pts',(-19.4438538502091,4.54755559186186,-15.714328005503));
#14648=CARTESIAN_POINT('Ctrl Pts',(-19.4720583966136,3.64194990530234,-15.6793387997003));
#14649=CARTESIAN_POINT('Ctrl Pts',(-19.4908797533348,2.73541348832897,-15.6559072598279));
#14650=CARTESIAN_POINT('Ctrl Pts',(-19.5097011100559,1.82887707135561,-15.6324757199555));
#14651=CARTESIAN_POINT('Ctrl Pts',(-19.5191393000384,0.92140994008045,-15.6206018131959));
#14652=CARTESIAN_POINT('Ctrl Pts',(-19.5192292333076,0.0130267934213882,
-15.6204894333562));
#14653=CARTESIAN_POINT('Ctrl Pts',(-19.5192296032355,0.00929028666506758,
-15.6204889710975));
#14654=CARTESIAN_POINT('Ctrl Pts',(-19.5192298134397,0.0055537642579053,
-15.6204887085208));
#14655=CARTESIAN_POINT('Ctrl Pts',(-19.5192298639648,0.0018172286253885,
-15.6204886455658));
#14656=CARTESIAN_POINT('Ctrl Pts',(-19.5192348828353,-0.369348115401582,
-15.6204823919898));
#14657=CARTESIAN_POINT('Ctrl Pts',(-19.5176643582502,-0.742191948960099,
-15.6224458020841));
#14658=CARTESIAN_POINT('Ctrl Pts',(-19.5145222635014,-1.11439334044658,
-15.6263694993203));
#14659=CARTESIAN_POINT('Ctrl Pts',(-19.5138140224602,-1.19828906037605,
-15.6272539167673));
#14660=CARTESIAN_POINT('Ctrl Pts',(-19.5130259293773,-1.2821519315032,-15.6282379367204));
#14661=CARTESIAN_POINT('Ctrl Pts',(-19.5121580206301,-1.36595500125534,
-15.6293214624937));
#14662=CARTESIAN_POINT('Ctrl Pts',(-19.5074230252224,-1.82315416151734,
-15.6352327862095));
#14663=CARTESIAN_POINT('Ctrl Pts',(-19.5003166417668,-2.27969557163659,
-15.6441004685152));
#14664=CARTESIAN_POINT('Ctrl Pts',(-19.4908482971583,-2.73568903694017,
-15.6558881146102));
#14665=CARTESIAN_POINT('Ctrl Pts',(-19.4720570197323,-3.64067296657114,
-15.6792823759227));
#14666=CARTESIAN_POINT('Ctrl Pts',(-19.4439717335206,-4.54350017251021,
-15.7141810578403));
#14667=CARTESIAN_POINT('Ctrl Pts',(-19.4065533265704,-5.44501179353637,
-15.7602565963606));
#14668=CARTESIAN_POINT('Ctrl Pts',(-19.3696896813279,-6.33315768985542,
-15.8056490233721));
#14669=CARTESIAN_POINT('Ctrl Pts',(-19.3237923792374,-7.22002942330059,
-15.8618979160963));
#14670=CARTESIAN_POINT('Ctrl Pts',(-19.268630719331,-8.1064004316186,-15.9286257991776));
#14671=CARTESIAN_POINT('Ctrl Pts',(-19.2345270546457,-8.65439880051663,
-15.969880274725));
#14672=CARTESIAN_POINT('Ctrl Pts',(-19.1968812804388,-9.20220540462824,
-16.0151404436434));
#14673=CARTESIAN_POINT('Ctrl Pts',(-19.1556295034202,-9.75000000012816,
-16.0643182664888));
#14674=CARTESIAN_POINT('',(19.1556241815518,-9.75000000004565,-16.0643138034269));
#14675=CARTESIAN_POINT('Origin',(0.,-9.75,0.));
#14676=CARTESIAN_POINT('',(19.1556296640198,9.75000000013388,-16.0643184011734));
#14677=CARTESIAN_POINT('Ctrl Pts',(19.1556295034199,-9.75000000013029,-16.0643182664893));
#14678=CARTESIAN_POINT('Ctrl Pts',(19.2223530215835,-8.86395859090214,-15.9847746057545));
#14679=CARTESIAN_POINT('Ctrl Pts',(19.2796449976598,-7.97788652210568,-15.9154801855084));
#14680=CARTESIAN_POINT('Ctrl Pts',(19.3277664720456,-7.09102032943713,-15.8568081429397));
#14681=CARTESIAN_POINT('Ctrl Pts',(19.3575175462091,-6.54271581034458,-15.8205341859993));
#14682=CARTESIAN_POINT('Ctrl Pts',(19.3837623989102,-5.99410748762773,-15.7883204384884));
#14683=CARTESIAN_POINT('Ctrl Pts',(19.4065533265683,-5.44501179353533,-15.7602565963632));
#14684=CARTESIAN_POINT('Ctrl Pts',(19.4439717335214,-4.54350017251043,-15.7141810578394));
#14685=CARTESIAN_POINT('Ctrl Pts',(19.4720570197304,-3.64067296657162,-15.6792823759249));
#14686=CARTESIAN_POINT('Ctrl Pts',(19.4908482971575,-2.73568903693967,-15.6558881146111));
#14687=CARTESIAN_POINT('Ctrl Pts',(19.5003166417666,-2.27969557163557,-15.6441004685155));
#14688=CARTESIAN_POINT('Ctrl Pts',(19.507423025222,-1.82315416151661,-15.6352327862101));
#14689=CARTESIAN_POINT('Ctrl Pts',(19.5121580206299,-1.36595500125495,-15.629321462494));
#14690=CARTESIAN_POINT('Ctrl Pts',(19.5160084774074,-0.994164650117414,
-15.6245144258432));
#14691=CARTESIAN_POINT('Ctrl Pts',(19.5182880791429,-0.621201496409886,
-15.6216657746395));
#14692=CARTESIAN_POINT('Ctrl Pts',(19.5189931473135,-0.249398212559946,
-15.6207845393862));
#14693=CARTESIAN_POINT('Ctrl Pts',(19.5191520725705,-0.165592227709809,
-15.6205859053464));
#14694=CARTESIAN_POINT('Ctrl Pts',(19.5192309952388,-0.0818449619717695,
-15.6204872359842));
#14695=CARTESIAN_POINT('Ctrl Pts',(19.5192298639648,0.00181722862345685,
-15.6204886455658));
#14696=CARTESIAN_POINT('Ctrl Pts',(19.5192298134397,0.00555376425672661,
-15.6204887085208));
#14697=CARTESIAN_POINT('Ctrl Pts',(19.5192296032355,0.00929028666463934,
-15.6204889710975));
#14698=CARTESIAN_POINT('Ctrl Pts',(19.5192292333076,0.0130267934217134,
-15.6204894333562));
#14699=CARTESIAN_POINT('Ctrl Pts',(19.5191393000384,0.921409940080897,-15.6206018131959));
#14700=CARTESIAN_POINT('Ctrl Pts',(19.5097011100581,1.82887707135682,-15.6324757199528));
#14701=CARTESIAN_POINT('Ctrl Pts',(19.4908797533385,2.73541348833066,-15.6559072598234));
#14702=CARTESIAN_POINT('Ctrl Pts',(19.4720583966188,3.6419499053045,-15.6793387996939));
#14703=CARTESIAN_POINT('Ctrl Pts',(19.4438538502151,4.54755559186421,-15.7143280054956));
#14704=CARTESIAN_POINT('Ctrl Pts',(19.4062538058678,5.45223695733326,-15.7606254070823));
#14705=CARTESIAN_POINT('Ctrl Pts',(19.370132545756,6.32133781845157,-15.8051019632736));
#14706=CARTESIAN_POINT('Ctrl Pts',(19.325339443103,7.18958919548238,-15.8599999935407));
#14707=CARTESIAN_POINT('Ctrl Pts',(19.2716949593314,8.05701156886618,-15.9249190639256));
#14708=CARTESIAN_POINT('Ctrl Pts',(19.2367733154138,8.62168873825368,-15.9671802714169));
#14709=CARTESIAN_POINT('Ctrl Pts',(19.1981008001052,9.1860149588975,-16.0136872060053));
#14710=CARTESIAN_POINT('Ctrl Pts',(19.1556296640198,9.75000000013389,-16.0643184011734));
#14711=CARTESIAN_POINT('Origin',(0.,9.75,0.));
#14712=CARTESIAN_POINT('Origin',(0.,10.75,0.));
#14713=CARTESIAN_POINT('',(18.3893975112944,10.75,-15.4217398231068));
#14714=CARTESIAN_POINT('',(16.4780203712833,10.75,-17.8656547184434));
#14715=CARTESIAN_POINT('Ctrl Pts',(18.3893975112944,10.75,-15.4217398231068));
#14716=CARTESIAN_POINT('Ctrl Pts',(17.7244634951049,10.75,-16.214629346884));
#14717=CARTESIAN_POINT('Ctrl Pts',(17.0876222525083,10.75,-17.0294901288799));
#14718=CARTESIAN_POINT('Ctrl Pts',(16.478020371287,10.75,-17.8656547184383));
#14719=CARTESIAN_POINT('',(4.08240831242321E-16,10.75,-25.));
#14720=CARTESIAN_POINT('Ctrl Pts',(16.4780203712861,10.75,-17.8656547184465));
#14721=CARTESIAN_POINT('Ctrl Pts',(16.4205369211924,10.75,-17.9445022924812));
#14722=CARTESIAN_POINT('Ctrl Pts',(16.3614956607445,10.75,-18.0219137128354));
#14723=CARTESIAN_POINT('Ctrl Pts',(16.3008084559825,10.75,-18.0978225947332));
#14724=CARTESIAN_POINT('Ctrl Pts',(16.2401227350897,10.75,-18.173729620575));
#14725=CARTESIAN_POINT('Ctrl Pts',(16.1778528394289,10.75,-18.2481856138866));
#14726=CARTESIAN_POINT('Ctrl Pts',(16.1143503256155,10.75,-18.321511971579));
#14727=CARTESIAN_POINT('Ctrl Pts',(15.9879798174003,10.7499999999999,-18.4674320073492));
#14728=CARTESIAN_POINT('Ctrl Pts',(15.8568594587015,10.7499999999999,-18.6089990995592));
#14729=CARTESIAN_POINT('Ctrl Pts',(15.7224917977638,10.7499999999988,-18.7475834112698));
#14730=CARTESIAN_POINT('Ctrl Pts',(15.7218180802141,10.7499999999988,-18.7482782710468));
#14731=CARTESIAN_POINT('Ctrl Pts',(15.7211442809102,10.7499999999988,-18.7489730559038));
#14732=CARTESIAN_POINT('Ctrl Pts',(15.7204704000415,10.7499999999988,-18.7496677660139));
#14733=CARTESIAN_POINT('Ctrl Pts',(15.451667324727,10.7499999999965,-19.0267793783135));
#14734=CARTESIAN_POINT('Ctrl Pts',(15.1690227653331,10.7500000000022,-19.2927577243446));
#14735=CARTESIAN_POINT('Ctrl Pts',(14.8798428323191,10.7499999999975,-19.5474336688286));
#14736=CARTESIAN_POINT('Ctrl Pts',(14.8783928927866,10.7499999999974,-19.5487106063949));
#14737=CARTESIAN_POINT('Ctrl Pts',(14.8769427885263,10.7499999999974,-19.5499872599372));
#14738=CARTESIAN_POINT('Ctrl Pts',(14.8754925204573,10.7499999999974,-19.5512636294347));
#14739=CARTESIAN_POINT('Ctrl Pts',(14.2970016154696,10.7499999999879,-20.0603889156465));
#14740=CARTESIAN_POINT('Ctrl Pts',(13.6908620621195,10.7500000000124,-20.5261584715322));
#14741=CARTESIAN_POINT('Ctrl Pts',(13.0629303706253,10.7499999999841,-20.957705974607));
#14742=CARTESIAN_POINT('Ctrl Pts',(13.0597819615603,10.7499999999839,-20.9598697259976));
#14743=CARTESIAN_POINT('Ctrl Pts',(13.0566330040481,10.7499999999838,-20.9620326166144));
#14744=CARTESIAN_POINT('Ctrl Pts',(13.0534834988268,10.7499999999836,-20.9641946476136));
#14745=CARTESIAN_POINT('Ctrl Pts',(12.4269079271698,10.7499999999561,-21.3943180206715));
#14746=CARTESIAN_POINT('Ctrl Pts',(11.7782352837989,10.7500000000018,-21.7897586824007));
#14747=CARTESIAN_POINT('Ctrl Pts',(11.1089027616845,10.7499999999977,-22.1527729443761));
#14748=CARTESIAN_POINT('Ctrl Pts',(11.103856085206,10.7499999999977,-22.1555100226993));
#14749=CARTESIAN_POINT('Ctrl Pts',(11.0988082712334,10.7499999999976,-22.1582452363645));
#14750=CARTESIAN_POINT('Ctrl Pts',(11.0937593195539,10.7499999999976,-22.1609785868902));
#14751=CARTESIAN_POINT('Ctrl Pts',(10.7597836855235,10.7499999999956,-22.341782946449));
#14752=CARTESIAN_POINT('Ctrl Pts',(10.4203659800424,10.7499999999967,-22.5145993685236));
#14753=CARTESIAN_POINT('Ctrl Pts',(10.075955307883,10.7499999999979,-22.6792702920911));
#14754=CARTESIAN_POINT('Ctrl Pts',(9.73154463572366,10.7499999999991,-22.8439412156585));
#14755=CARTESIAN_POINT('Ctrl Pts',(9.38214027285201,10.7499999999998,-23.0004669395086));
#14756=CARTESIAN_POINT('Ctrl Pts',(9.02816344904727,10.7499999999999,-23.148638564313));
#14757=CARTESIAN_POINT('Ctrl Pts',(9.02106352923122,10.7499999999999,-23.1516105290982));
#14758=CARTESIAN_POINT('Ctrl Pts',(9.01396146848508,10.7499999999999,-23.1545792568972));
#14759=CARTESIAN_POINT('Ctrl Pts',(9.00685727508312,10.7499999999999,-23.1575447426818));
#14760=CARTESIAN_POINT('Ctrl Pts',(8.69609748902353,10.75,-23.287264427359));
#14761=CARTESIAN_POINT('Ctrl Pts',(8.38265057292746,10.75,-23.4103036057306));
#14762=CARTESIAN_POINT('Ctrl Pts',(8.06678449157996,10.75,-23.5265460693149));
#14763=CARTESIAN_POINT('Ctrl Pts',(7.74909985495579,10.75,-23.6434577828062));
#14764=CARTESIAN_POINT('Ctrl Pts',(7.4289681233337,10.75,-23.7534943162534));
#14765=CARTESIAN_POINT('Ctrl Pts',(7.10667522874612,10.75,-23.8565884582872));
#14766=CARTESIAN_POINT('Ctrl Pts',(7.02075621786697,10.75,-23.8840719891367));
#14767=CARTESIAN_POINT('Ctrl Pts',(6.93468368892621,10.75,-23.911062412747));
#14768=CARTESIAN_POINT('Ctrl Pts',(6.84846321645907,10.75,-23.9375590587731));
#14769=CARTESIAN_POINT('Ctrl Pts',(6.47917928205354,10.75,-24.0510447010236));
#14770=CARTESIAN_POINT('Ctrl Pts',(6.10762958554647,10.75,-24.155334970232));
#14771=CARTESIAN_POINT('Ctrl Pts',(5.73386157021048,10.75,-24.2505804378535));
#14772=CARTESIAN_POINT('Ctrl Pts',(5.3600935548745,10.75,-24.3458259054749));
#14773=CARTESIAN_POINT('Ctrl Pts',(4.98410756392965,10.75,-24.4320267971511));
#14774=CARTESIAN_POINT('Ctrl Pts',(4.6059333896843,10.75,-24.5093375099453));
#14775=CARTESIAN_POINT('Ctrl Pts',(4.60558352323334,10.75,-24.5094090336678));
#14776=CARTESIAN_POINT('Ctrl Pts',(4.60523365489507,10.75,-24.5094805497838));
#14777=CARTESIAN_POINT('Ctrl Pts',(4.60488378466999,10.75,-24.5095520582932));
#14778=CARTESIAN_POINT('Ctrl Pts',(4.29775236332103,10.75,-24.5723253626734));
#14779=CARTESIAN_POINT('Ctrl Pts',(3.98912819460999,10.75,-24.6291799941854));
#14780=CARTESIAN_POINT('Ctrl Pts',(3.67936135400966,10.75,-24.6800307868044));
#14781=CARTESIAN_POINT('Ctrl Pts',(3.37064081951635,10.7499999999999,-24.7307098196095));
#14782=CARTESIAN_POINT('Ctrl Pts',(3.06078535062693,10.7499999999999,-24.775425478857));
#14783=CARTESIAN_POINT('Ctrl Pts',(2.75015409326968,10.7499999999996,-24.814143692227));
#14784=CARTESIAN_POINT('Ctrl Pts',(2.60693647555524,10.7499999999995,-24.8319948586814));
#14785=CARTESIAN_POINT('Ctrl Pts',(2.46355412155261,10.7499999999993,-24.8485718507124));
#14786=CARTESIAN_POINT('Ctrl Pts',(2.32004310769269,10.7499999999991,-24.8638749604557));
#14787=CARTESIAN_POINT('Ctrl Pts',(2.31835963494414,10.7499999999991,-24.8640544753761));
#14788=CARTESIAN_POINT('Ctrl Pts',(2.31667617442673,10.7499999999991,-24.8642338083549));
#14789=CARTESIAN_POINT('Ctrl Pts',(2.31499272620476,10.7499999999991,-24.8644129594266));
#14790=CARTESIAN_POINT('Ctrl Pts',(1.70961577407402,10.7499999999982,-24.9288366395314));
#14791=CARTESIAN_POINT('Ctrl Pts',(1.10236193375945,10.75,-24.9700975683441));
#14792=CARTESIAN_POINT('Ctrl Pts',(0.493954693746763,10.75,-24.9892687909964));
#14793=CARTESIAN_POINT('Ctrl Pts',(0.386484823791873,10.75,-24.9926552214493));
#14794=CARTESIAN_POINT('Ctrl Pts',(0.278978971249718,10.75,-24.9953525365432));
#14795=CARTESIAN_POINT('Ctrl Pts',(0.171441131934135,10.75,-24.9973668172451));
#14796=CARTESIAN_POINT('Ctrl Pts',(0.114302919084394,10.75,-24.9984370674957));
#14797=CARTESIAN_POINT('Ctrl Pts',(0.0571556757661779,10.75,-24.9993144879768));
#14798=CARTESIAN_POINT('Ctrl Pts',(6.03940677783316E-16,10.75,-25.));
#14799=CARTESIAN_POINT('',(-16.4780203712963,10.75,-17.8656547184255));
#14800=CARTESIAN_POINT('Ctrl Pts',(8.88178419700125E-16,10.75,-25.));
#14801=CARTESIAN_POINT('Ctrl Pts',(-0.631893351362637,10.75,-24.992420407891));
#14802=CARTESIAN_POINT('Ctrl Pts',(-1.26314073990296,10.75,-24.9608795160537));
#14803=CARTESIAN_POINT('Ctrl Pts',(-1.89206141815216,10.75,-24.9051003815217));
#14804=CARTESIAN_POINT('Ctrl Pts',(-2.03226925017558,10.75,-24.8926653133242));
#14805=CARTESIAN_POINT('Ctrl Pts',(-2.17236144346044,10.75,-24.8790258193833));
#14806=CARTESIAN_POINT('Ctrl Pts',(-2.31231938275716,10.75,-24.864179185895));
#14807=CARTESIAN_POINT('Ctrl Pts',(-2.93636235324608,10.75,-24.7979811744756));
#14808=CARTESIAN_POINT('Ctrl Pts',(-3.55773440824655,10.75,-24.7077804387484));
#14809=CARTESIAN_POINT('Ctrl Pts',(-4.17479133535945,10.75,-24.5933678196603));
#14810=CARTESIAN_POINT('Ctrl Pts',(-4.31689719651806,10.75,-24.5670190290569));
#14811=CARTESIAN_POINT('Ctrl Pts',(-4.45877423678966,10.75,-24.5393863433226));
#14812=CARTESIAN_POINT('Ctrl Pts',(-4.60040245249664,10.75,-24.5104675943794));
#14813=CARTESIAN_POINT('Ctrl Pts',(-4.60074315414983,10.75,-24.5103980272701));
#14814=CARTESIAN_POINT('Ctrl Pts',(-4.60108385438549,10.75,-24.5103284527139));
#14815=CARTESIAN_POINT('Ctrl Pts',(-4.60142455320338,10.75,-24.5102588707109));
#14816=CARTESIAN_POINT('Ctrl Pts',(-5.27342211797078,10.75,-24.3730146711527));
#14817=CARTESIAN_POINT('Ctrl Pts',(-5.93871948223922,10.75,-24.2073770139159));
#14818=CARTESIAN_POINT('Ctrl Pts',(-6.59553787934151,10.75,-24.0134739845937));
#14819=CARTESIAN_POINT('Ctrl Pts',(-7.24524697488622,10.75,-23.8216697319112));
#14820=CARTESIAN_POINT('Ctrl Pts',(-7.88666018322436,10.75,-23.6022085437364));
#14821=CARTESIAN_POINT('Ctrl Pts',(-8.51803988731519,10.75,-23.3551660550721));
#14822=CARTESIAN_POINT('Ctrl Pts',(-8.68535124885221,10.75,-23.2897014624219));
#14823=CARTESIAN_POINT('Ctrl Pts',(-8.85195793187626,10.75,-23.2222998119581));
#14824=CARTESIAN_POINT('Ctrl Pts',(-9.01782734025242,10.75,-23.1529619510151));
#14825=CARTESIAN_POINT('Ctrl Pts',(-9.01859758920051,10.75,-23.1526399662984));
#14826=CARTESIAN_POINT('Ctrl Pts',(-9.01936782291524,10.75,-23.1523179395502));
#14827=CARTESIAN_POINT('Ctrl Pts',(-9.02013804139308,10.75,-23.1519958707704));
#14828=CARTESIAN_POINT('Ctrl Pts',(-9.73165202060789,10.75,-22.8544745236052));
#14829=CARTESIAN_POINT('Ctrl Pts',(-10.4267722486049,10.75,-22.5225508541856));
#14830=CARTESIAN_POINT('Ctrl Pts',(-11.1049075898659,10.75,-22.1549367784204));
#14831=CARTESIAN_POINT('Ctrl Pts',(-11.1050463232738,10.75,-22.1548615716727));
#14832=CARTESIAN_POINT('Ctrl Pts',(-11.1051850560842,10.75,-22.1547863633518));
#14833=CARTESIAN_POINT('Ctrl Pts',(-11.105323788297,10.75,-22.1547111534577));
#14834=CARTESIAN_POINT('Ctrl Pts',(-11.4745607689731,10.75,-21.9545393718602));
#14835=CARTESIAN_POINT('Ctrl Pts',(-11.8388346073417,10.7499999999999,-21.7436243514817));
#14836=CARTESIAN_POINT('Ctrl Pts',(-12.196154206087,10.7499999999996,-21.5227465720604));
#14837=CARTESIAN_POINT('Ctrl Pts',(-12.4953092091938,10.7499999999994,-21.3378233464075));
#14838=CARTESIAN_POINT('Ctrl Pts',(-12.7895904599738,10.7499999999992,-21.1459156366744));
#14839=CARTESIAN_POINT('Ctrl Pts',(-13.0778256121902,10.7499999999995,-20.9474537314311));
#14840=CARTESIAN_POINT('Ctrl Pts',(-13.0784156919486,10.7499999999995,-20.9470474369448));
#14841=CARTESIAN_POINT('Ctrl Pts',(-13.0790057477787,10.7499999999995,-20.9466411152569));
#14842=CARTESIAN_POINT('Ctrl Pts',(-13.0795957796768,10.7499999999995,-20.9462347663615));
#14843=CARTESIAN_POINT('Ctrl Pts',(-13.7123512511636,10.7500000000004,-20.5104625857627));
#14844=CARTESIAN_POINT('Ctrl Pts',(-14.3179636229281,10.7499999999992,-20.0431451182884));
#14845=CARTESIAN_POINT('Ctrl Pts',(-14.8908179209084,10.7499999999998,-19.5377573520794));
#14846=CARTESIAN_POINT('Ctrl Pts',(-14.891085008639,10.7499999999998,-19.5375217199615));
#14847=CARTESIAN_POINT('Ctrl Pts',(-14.8913520892958,10.7499999999998,-19.5372860796229));
#14848=CARTESIAN_POINT('Ctrl Pts',(-14.8916191628765,10.7499999999998,-19.5370504310607));
#14849=CARTESIAN_POINT('Ctrl Pts',(-15.1780311374702,10.7500000000001,-19.284338912937));
#14850=CARTESIAN_POINT('Ctrl Pts',(-15.4563063216582,10.7499999999999,-19.022171134779));
#14851=CARTESIAN_POINT('Ctrl Pts',(-15.7232342401124,10.75,-18.7468157768201));
#14852=CARTESIAN_POINT('Ctrl Pts',(-15.7233586926443,10.75,-18.746687395077));
#14853=CARTESIAN_POINT('Ctrl Pts',(-15.7234831427055,10.75,-18.7465590104624));
#14854=CARTESIAN_POINT('Ctrl Pts',(-15.7236075902949,10.75,-18.7464306229752));
#14855=CARTESIAN_POINT('Ctrl Pts',(-15.8570635065209,10.75,-18.6087496134541));
#14856=CARTESIAN_POINT('Ctrl Pts',(-15.9876823298412,10.75,-18.4677594530587));
#14857=CARTESIAN_POINT('Ctrl Pts',(-16.1140602454271,10.75,-18.3218466327017));
#14858=CARTESIAN_POINT('Ctrl Pts',(-16.1773091023549,10.75,-18.2488210644612));
#14859=CARTESIAN_POINT('Ctrl Pts',(-16.2394660158614,10.75,-18.1745279741513));
#14860=CARTESIAN_POINT('Ctrl Pts',(-16.300199402483,10.75,-18.0985842575497));
#14861=CARTESIAN_POINT('Ctrl Pts',(-16.3609359034934,10.75,-18.0226366465785));
#14862=CARTESIAN_POINT('Ctrl Pts',(-16.4201884779383,10.75,-17.94498023769));
#14863=CARTESIAN_POINT('Ctrl Pts',(-16.4780203712963,10.75,-17.8656547184255));
#14864=CARTESIAN_POINT('',(-18.3893975112961,10.75,-15.4217398231048));
#14865=CARTESIAN_POINT('Ctrl Pts',(-16.4780203712963,10.75,-17.8656547184255));
#14866=CARTESIAN_POINT('Ctrl Pts',(-17.0876222525177,10.75,-17.0294901288675));
#14867=CARTESIAN_POINT('Ctrl Pts',(-17.7244634951036,10.75,-16.2146293468709));
#14868=CARTESIAN_POINT('Ctrl Pts',(-18.3893975112961,10.75,-15.4217398231048));
#14869=CARTESIAN_POINT('Origin',(0.,10.75,0.));
#14870=CARTESIAN_POINT('Origin',(0.,-10.75,0.));
#14871=CARTESIAN_POINT('',(18.3893975112955,-10.75,-15.4217398231056));
#14872=CARTESIAN_POINT('',(-18.3893975112944,-10.75,-15.4217398231068));
#14873=CARTESIAN_POINT('Origin',(0.,-10.75,0.));
#14874=CARTESIAN_POINT('',(-16.4780203712963,-10.75,-17.8656547184255));
#14875=CARTESIAN_POINT('Ctrl Pts',(-18.3893975112945,-10.75,-15.4217398231068));
#14876=CARTESIAN_POINT('Ctrl Pts',(-17.7244634951085,-10.75,-16.2146293468773));
#14877=CARTESIAN_POINT('Ctrl Pts',(-17.0876222525172,-10.75,-17.0294901288682));
#14878=CARTESIAN_POINT('Ctrl Pts',(-16.4780203712963,-10.75,-17.8656547184255));
#14879=CARTESIAN_POINT('',(0.,-10.75,-25.));
#14880=CARTESIAN_POINT('Ctrl Pts',(-16.4780203712963,-10.75,-17.8656547184255));
#14881=CARTESIAN_POINT('Ctrl Pts',(-16.4201493510906,-10.75,-17.9450339063976));
#14882=CARTESIAN_POINT('Ctrl Pts',(-16.360820089721,-10.75,-18.0227902935397));
#14883=CARTESIAN_POINT('Ctrl Pts',(-16.2999644844546,-10.75,-18.0988780799066));
#14884=CARTESIAN_POINT('Ctrl Pts',(-16.2391116407599,-10.75,-18.1749624134795));
#14885=CARTESIAN_POINT('Ctrl Pts',(-16.1767937814564,-10.75,-18.2494353360594));
#14886=CARTESIAN_POINT('Ctrl Pts',(-16.1133493511491,-10.7499999999999,
-18.3226679211682));
#14887=CARTESIAN_POINT('Ctrl Pts',(-15.9876961209516,-10.7499999999997,
-18.467706828919));
#14888=CARTESIAN_POINT('Ctrl Pts',(-15.857743766938,-10.7499999999996,-18.6080126030319));
#14889=CARTESIAN_POINT('Ctrl Pts',(-15.724890365442,-10.7499999999952,-18.7451110957646));
#14890=CARTESIAN_POINT('Ctrl Pts',(-15.7235857860446,-10.7499999999952,
-18.7464573606476));
#14891=CARTESIAN_POINT('Ctrl Pts',(-15.7222809262691,-10.7499999999952,
-18.7478033165219));
#14892=CARTESIAN_POINT('Ctrl Pts',(-15.7209757874349,-10.7499999999951,
-18.749148964841));
#14893=CARTESIAN_POINT('Ctrl Pts',(-15.4551501413287,-10.7499999999865,
-19.02322542666));
#14894=CARTESIAN_POINT('Ctrl Pts',(-15.177768808186,-10.750000000015,-19.2845652736965));
#14895=CARTESIAN_POINT('Ctrl Pts',(-14.8920303997885,-10.7499999999828,
-19.5366947908981));
#14896=CARTESIAN_POINT('Ctrl Pts',(-14.8892245807239,-10.7499999999825,
-19.5391705861897));
#14897=CARTESIAN_POINT('Ctrl Pts',(-14.8864179605812,-10.7499999999821,
-19.5416454867311));
#14898=CARTESIAN_POINT('Ctrl Pts',(-14.8836105423087,-10.7499999999818,
-19.5441194959428));
#14899=CARTESIAN_POINT('Ctrl Pts',(-14.5626185949198,-10.7499999999458,
-19.826990432017));
#14900=CARTESIAN_POINT('Ctrl Pts',(-14.2310028354858,-10.7499999999655,
-20.0982233034529));
#14901=CARTESIAN_POINT('Ctrl Pts',(-13.8898057176469,-10.7499999999759,
-20.358849639778));
#14902=CARTESIAN_POINT('Ctrl Pts',(-13.6232076047817,-10.749999999984,-20.5624928881951));
#14903=CARTESIAN_POINT('Ctrl Pts',(-13.3507587393612,-10.7499999999906,
-20.7596595859911));
#14904=CARTESIAN_POINT('Ctrl Pts',(-13.0729414760137,-10.7499999999578,
-20.9508259365018));
#14905=CARTESIAN_POINT('Ctrl Pts',(-13.0667248663834,-10.7499999999571,
-20.9551035921135));
#14906=CARTESIAN_POINT('Ctrl Pts',(-13.0605051235057,-10.7499999999564,
-20.9593785431024));
#14907=CARTESIAN_POINT('Ctrl Pts',(-13.0542822577895,-10.7499999999557,
-20.9636507892648));
#14908=CARTESIAN_POINT('Ctrl Pts',(-12.8276147931846,-10.7499999999303,
-21.1192670679927));
#14909=CARTESIAN_POINT('Ctrl Pts',(-12.5979370989195,-10.7499999999392,
-21.2704240340891));
#14910=CARTESIAN_POINT('Ctrl Pts',(-12.365564761205,-10.7499999999554,-21.4170600650478));
#14911=CARTESIAN_POINT('Ctrl Pts',(-12.1277109810229,-10.749999999972,-21.5671551005305));
#14912=CARTESIAN_POINT('Ctrl Pts',(-11.8870339411185,-10.7499999999879,
-21.7125134564541));
#14913=CARTESIAN_POINT('Ctrl Pts',(-11.6438956109018,-10.7499999999931,
-21.8531191015724));
#14914=CARTESIAN_POINT('Ctrl Pts',(-11.4634201196036,-10.749999999997,-21.9574871494215));
#14915=CARTESIAN_POINT('Ctrl Pts',(-11.2815890286072,-10.7499999999978,
-22.0592376569264));
#14916=CARTESIAN_POINT('Ctrl Pts',(-11.0985582855635,-10.7499999999957,
-22.158380780832));
#14917=CARTESIAN_POINT('Ctrl Pts',(-11.0924596370167,-10.7499999999956,
-22.1616842644898));
#14918=CARTESIAN_POINT('Ctrl Pts',(-11.0863595888253,-10.7499999999955,
-22.1649848892748));
#14919=CARTESIAN_POINT('Ctrl Pts',(-11.0802581423629,-10.7499999999955,
-22.168282658021));
#14920=CARTESIAN_POINT('Ctrl Pts',(-10.4089256243362,-10.7499999999882,
-22.5311309448827));
#14921=CARTESIAN_POINT('Ctrl Pts',(-9.7205987275344,-10.7500000000003,-22.8592637055778));
#14922=CARTESIAN_POINT('Ctrl Pts',(-9.0158247965325,-10.7499999999996,-23.1537997929039));
#14923=CARTESIAN_POINT('Ctrl Pts',(-9.01167151414176,-10.7499999999996,
-23.1555355148015));
#14924=CARTESIAN_POINT('Ctrl Pts',(-9.00751768000453,-10.7499999999996,
-23.1572700615062));
#14925=CARTESIAN_POINT('Ctrl Pts',(-9.0033632951643,-10.7499999999996,-23.1590034328983));
#14926=CARTESIAN_POINT('Ctrl Pts',(-8.71652133934044,-10.7499999999993,
-23.2786850847921));
#14927=CARTESIAN_POINT('Ctrl Pts',(-8.42699173100363,-10.7499999999994,
-23.3927719037949));
#14928=CARTESIAN_POINT('Ctrl Pts',(-8.13515127880793,-10.7499999999996,
-23.5011251356437));
#14929=CARTESIAN_POINT('Ctrl Pts',(-7.84327400478459,-10.7499999999998,
-23.6094920385378));
#14930=CARTESIAN_POINT('Ctrl Pts',(-7.549085393291,-10.7499999999999,-23.7121238639655));
#14931=CARTESIAN_POINT('Ctrl Pts',(-7.25298387983204,-10.7499999999999,
-23.8089293460351));
#14932=CARTESIAN_POINT('Ctrl Pts',(-7.11519835173526,-10.7499999999999,
-23.8539760407103));
#14933=CARTESIAN_POINT('Ctrl Pts',(-6.97699891083036,-10.7499999999999,
-23.8977618104917));
#14934=CARTESIAN_POINT('Ctrl Pts',(-6.8384272034732,-10.7499999999999,-23.9402810023015));
#14935=CARTESIAN_POINT('Ctrl Pts',(-6.83474659856658,-10.7499999999999,
-23.9414103551037));
#14936=CARTESIAN_POINT('Ctrl Pts',(-6.83106554363849,-10.7499999999999,
-23.9425388719248));
#14937=CARTESIAN_POINT('Ctrl Pts',(-6.8273840387324,-10.7499999999999,-23.9436665526118));
#14938=CARTESIAN_POINT('Ctrl Pts',(-6.09245639192048,-10.7499999999998,
-24.1687820243408));
#14939=CARTESIAN_POINT('Ctrl Pts',(-5.34937233574249,-10.7500000000001,
-24.3576172870069));
#14940=CARTESIAN_POINT('Ctrl Pts',(-4.59800314866546,-10.7499999999998,
-24.5109577875767));
#14941=CARTESIAN_POINT('Ctrl Pts',(-4.59383852606573,-10.7499999999998,
-24.5118077097257));
#14942=CARTESIAN_POINT('Ctrl Pts',(-4.58967362230916,-10.7499999999998,
-24.5126565466446));
#14943=CARTESIAN_POINT('Ctrl Pts',(-4.585508438488,-10.7499999999998,-24.5135042982985));
#14944=CARTESIAN_POINT('Ctrl Pts',(-4.23868940594231,-10.7499999999997,
-24.5840933577707));
#14945=CARTESIAN_POINT('Ctrl Pts',(-3.8899125665333,-10.7500000007398,-24.6471311889045));
#14946=CARTESIAN_POINT('Ctrl Pts',(-3.53980407982917,-10.7499999989718,
-24.7025066732745));
#14947=CARTESIAN_POINT('Ctrl Pts',(-3.20653186901385,-10.7499999972888,
-24.75521922039));
#14948=CARTESIAN_POINT('Ctrl Pts',(-2.87205245696364,-10.7499999917215,
-24.8009885036796));
#14949=CARTESIAN_POINT('Ctrl Pts',(-2.53691289996853,-10.7499999750427,
-24.8397660990454));
#14950=CARTESIAN_POINT('Ctrl Pts',(-2.4616811610157,-10.7499999712987,-24.8484708486665));
#14951=CARTESIAN_POINT('Ctrl Pts',(-2.38641620209076,-10.7499999670649,
-24.8568234837151));
#14952=CARTESIAN_POINT('Ctrl Pts',(-2.3111242988961,-10.7499999624566,-24.8648238156686));
#14953=CARTESIAN_POINT('Ctrl Pts',(-1.9274828828541,-10.7499999389757,-24.905588606426));
#14954=CARTESIAN_POINT('Ctrl Pts',(-1.54279117061237,-10.7499999002255,
-24.9372493539721));
#14955=CARTESIAN_POINT('Ctrl Pts',(-1.15724985369559,-10.7499999035675,
-24.95979124596));
#14956=CARTESIAN_POINT('Ctrl Pts',(-1.01440345966211,-10.7499999048058,
-24.9681432119981));
#14957=CARTESIAN_POINT('Ctrl Pts',(-0.871510359726857,-10.7499999153928,
-24.9752345292119));
#14958=CARTESIAN_POINT('Ctrl Pts',(-0.728466427406036,-10.7499999352919,
-24.9810597553893));
#14959=CARTESIAN_POINT('Ctrl Pts',(-0.678473124110684,-10.7499999422465,
-24.9830956494977));
#14960=CARTESIAN_POINT('Ctrl Pts',(-0.62846143143074,-10.7499999499415,
-24.9849773637484));
#14961=CARTESIAN_POINT('Ctrl Pts',(-0.578426969045136,-10.74999995742,-24.9867061497547));
#14962=CARTESIAN_POINT('Ctrl Pts',(-0.481828888224218,-10.7499999718582,
-24.9900437974959));
#14963=CARTESIAN_POINT('Ctrl Pts',(-0.385082356737824,-10.7499999859661,
-24.99280714982));
#14964=CARTESIAN_POINT('Ctrl Pts',(-0.288554981890424,-10.7499999930961,
-24.9950091292011));
#14965=CARTESIAN_POINT('Ctrl Pts',(-0.192027607043022,-10.750000000226,
-24.9972111085822));
#14966=CARTESIAN_POINT('Ctrl Pts',(-0.0957196018798722,-10.75,-24.9988519611205));
#14967=CARTESIAN_POINT('Ctrl Pts',(-5.35841952801743E-40,-10.75,-25.));
#14968=CARTESIAN_POINT('',(16.4780203712966,-10.75,-17.8656547184251));
#14969=CARTESIAN_POINT('Ctrl Pts',(0.,-10.75,-25.));
#14970=CARTESIAN_POINT('Ctrl Pts',(0.63189335421386,-10.75,-24.9924204078283));
#14971=CARTESIAN_POINT('Ctrl Pts',(1.26314074559829,-10.75,-24.9608795157349));
#14972=CARTESIAN_POINT('Ctrl Pts',(1.89206142666417,-10.75,-24.905100380736));
#14973=CARTESIAN_POINT('Ctrl Pts',(2.03226925584466,-10.75,-24.8926653127422));
#14974=CARTESIAN_POINT('Ctrl Pts',(2.17236144629095,-10.75,-24.8790258190543));
#14975=CARTESIAN_POINT('Ctrl Pts',(2.31231938275462,-10.75,-24.8641791858681));
#14976=CARTESIAN_POINT('Ctrl Pts',(2.93636235981245,-10.75,-24.7979811737587));
#14977=CARTESIAN_POINT('Ctrl Pts',(3.55773442132701,-10.75,-24.7077804368426));
#14978=CARTESIAN_POINT('Ctrl Pts',(4.17479135484504,-10.75,-24.5933678160459));
#14979=CARTESIAN_POINT('Ctrl Pts',(4.3168972094877,-10.75,-24.5670190265306));
#14980=CARTESIAN_POINT('Ctrl Pts',(4.4587742432633,-10.75,-24.5393863420014));
#14981=CARTESIAN_POINT('Ctrl Pts',(4.60040245249694,-10.75,-24.5104675943802));
#14982=CARTESIAN_POINT('Ctrl Pts',(4.60074315415015,-10.75,-24.5103980272708));
#14983=CARTESIAN_POINT('Ctrl Pts',(4.60108385438582,-10.75,-24.5103284527146));
#14984=CARTESIAN_POINT('Ctrl Pts',(4.60142455320371,-10.75,-24.5102588707117));
#14985=CARTESIAN_POINT('Ctrl Pts',(5.27342211902175,-10.75,-24.3730146709398));
#14986=CARTESIAN_POINT('Ctrl Pts',(5.93871948432097,-10.75,-24.2073770134027));
#14987=CARTESIAN_POINT('Ctrl Pts',(6.59553788242437,-10.75,-24.0134739836911));
#14988=CARTESIAN_POINT('Ctrl Pts',(7.24524697964132,-10.75,-23.8216697304222));
#14989=CARTESIAN_POINT('Ctrl Pts',(7.88666018960527,-10.75,-23.6022085415156));
#14990=CARTESIAN_POINT('Ctrl Pts',(8.51803989526079,-10.75,-23.3551660519723));
#14991=CARTESIAN_POINT('Ctrl Pts',(8.68535125412791,-10.75,-23.2897014602961));
#14992=CARTESIAN_POINT('Ctrl Pts',(8.85195793450375,-10.75,-23.2222998108673));
#14993=CARTESIAN_POINT('Ctrl Pts',(9.01782734025492,-10.75,-23.1529619510203));
#14994=CARTESIAN_POINT('Ctrl Pts',(9.01859758920301,-10.75,-23.1526399663036));
#14995=CARTESIAN_POINT('Ctrl Pts',(9.01936782291774,-10.75,-23.1523179395554));
#14996=CARTESIAN_POINT('Ctrl Pts',(9.02013804139559,-10.75,-23.1519958707756));
#14997=CARTESIAN_POINT('Ctrl Pts',(9.73165202060862,-10.75,-22.8544745236056));
#14998=CARTESIAN_POINT('Ctrl Pts',(10.4267722486079,-10.75,-22.5225508541904));
#14999=CARTESIAN_POINT('Ctrl Pts',(11.1049075898677,-10.75,-22.1549367784228));
#15000=CARTESIAN_POINT('Ctrl Pts',(11.1050463232755,-10.75,-22.1548615716751));
#15001=CARTESIAN_POINT('Ctrl Pts',(11.1051850560859,-10.75,-22.1547863633542));
#15002=CARTESIAN_POINT('Ctrl Pts',(11.1053237882988,-10.75,-22.1547111534601));
#15003=CARTESIAN_POINT('Ctrl Pts',(11.4745607700401,-10.75,-21.9545393712836));
#15004=CARTESIAN_POINT('Ctrl Pts',(11.8388346094455,-10.7499999999999,-21.7436243502645));
#15005=CARTESIAN_POINT('Ctrl Pts',(12.1961542091821,-10.7499999999996,-21.5227465701481));
#15006=CARTESIAN_POINT('Ctrl Pts',(12.4953092112239,-10.7499999999994,-21.3378233450845));
#15007=CARTESIAN_POINT('Ctrl Pts',(12.7895904609685,-10.7499999999992,-21.1459156359909));
#15008=CARTESIAN_POINT('Ctrl Pts',(13.0778256121919,-10.7499999999995,-20.9474537314328));
#15009=CARTESIAN_POINT('Ctrl Pts',(13.0784156919504,-10.7499999999995,-20.9470474369465));
#15010=CARTESIAN_POINT('Ctrl Pts',(13.0790057477804,-10.7499999999995,-20.9466411152586));
#15011=CARTESIAN_POINT('Ctrl Pts',(13.0795957796785,-10.7499999999995,-20.9462347663633));
#15012=CARTESIAN_POINT('Ctrl Pts',(13.712351251167,-10.7500000000004,-20.5104625857665));
#15013=CARTESIAN_POINT('Ctrl Pts',(14.3179636229283,-10.7499999999992,-20.043145118288));
#15014=CARTESIAN_POINT('Ctrl Pts',(14.8908179209099,-10.7499999999998,-19.5377573520803));
#15015=CARTESIAN_POINT('Ctrl Pts',(14.8910850086404,-10.7499999999998,-19.5375217199623));
#15016=CARTESIAN_POINT('Ctrl Pts',(14.8913520892973,-10.7499999999998,-19.5372860796237));
#15017=CARTESIAN_POINT('Ctrl Pts',(14.8916191628779,-10.7499999999998,-19.5370504310615));
#15018=CARTESIAN_POINT('Ctrl Pts',(15.1780311374723,-10.7500000000001,-19.2843389129384));
#15019=CARTESIAN_POINT('Ctrl Pts',(15.4563063216585,-10.7499999999999,-19.0221711347786));
#15020=CARTESIAN_POINT('Ctrl Pts',(15.723234240113,-10.75,-18.7468157768199));
#15021=CARTESIAN_POINT('Ctrl Pts',(15.7233586926449,-10.75,-18.7466873950767));
#15022=CARTESIAN_POINT('Ctrl Pts',(15.7234831427061,-10.75,-18.7465590104622));
#15023=CARTESIAN_POINT('Ctrl Pts',(15.7236075902955,-10.75,-18.746430622975));
#15024=CARTESIAN_POINT('Ctrl Pts',(15.8570635065216,-10.75,-18.6087496134539));
#15025=CARTESIAN_POINT('Ctrl Pts',(15.9876823298417,-10.75,-18.4677594530583));
#15026=CARTESIAN_POINT('Ctrl Pts',(16.1140602454275,-10.75,-18.3218466327013));
#15027=CARTESIAN_POINT('Ctrl Pts',(16.1773091023553,-10.75,-18.2488210644609));
#15028=CARTESIAN_POINT('Ctrl Pts',(16.2394660158614,-10.75,-18.1745279741503));
#15029=CARTESIAN_POINT('Ctrl Pts',(16.3001994024834,-10.75,-18.0985842575493));
#15030=CARTESIAN_POINT('Ctrl Pts',(16.360935903494,-10.75,-18.0226366465788));
#15031=CARTESIAN_POINT('Ctrl Pts',(16.4201884779384,-10.75,-17.9449802376892));
#15032=CARTESIAN_POINT('Ctrl Pts',(16.4780203712966,-10.75,-17.8656547184251));
#15033=CARTESIAN_POINT('Ctrl Pts',(16.4780203712966,-10.75,-17.8656547184251));
#15034=CARTESIAN_POINT('Ctrl Pts',(17.0876222525178,-10.75,-17.0294901288675));
#15035=CARTESIAN_POINT('Ctrl Pts',(17.7244634951146,-10.75,-16.2146293468808));
#15036=CARTESIAN_POINT('Ctrl Pts',(18.3893975112954,-10.75,-15.4217398231056));
#15037=CARTESIAN_POINT('',(-2.44929359829471E-15,-10.75,20.));
#15038=CARTESIAN_POINT('Origin',(0.,-10.75,0.));
#15039=CARTESIAN_POINT('Origin',(0.,0.,25.002));
#15040=CARTESIAN_POINT('',(10.75,0.,-61.5));
#15041=CARTESIAN_POINT('Origin',(0.,0.,-61.5));
#15042=CARTESIAN_POINT('',(10.7499999978076,1.45695088265319E-14,-40.6132670239265));
#15043=CARTESIAN_POINT('',(10.75,-1.3164953090834E-15,25.002));
#15044=CARTESIAN_POINT('',(10.5060622858799,-2.277093596059,-42.0119030751999));
#15045=CARTESIAN_POINT('Ctrl Pts',(10.7499999978076,2.23887749120318E-14,
-40.6132670239265));
#15046=CARTESIAN_POINT('Ctrl Pts',(10.7499999122695,-0.0543484520734741,
-40.6132674463034));
#15047=CARTESIAN_POINT('Ctrl Pts',(10.7495859465627,-0.108343313907444,
-40.6157107158717));
#15048=CARTESIAN_POINT('Ctrl Pts',(10.7487784221861,-0.161956425874147,
-40.620473106121));
#15049=CARTESIAN_POINT('Ctrl Pts',(10.748135179199,-0.204662577278424,-40.6242666437757));
#15050=CARTESIAN_POINT('Ctrl Pts',(10.7472420423001,-0.247126965572841,
-40.6295327410255));
#15051=CARTESIAN_POINT('Ctrl Pts',(10.7461054443956,-0.289340245956811,
-40.6362316036066));
#15052=CARTESIAN_POINT('Ctrl Pts',(10.7456145340568,-0.307572670717383,
-40.6391249231231));
#15053=CARTESIAN_POINT('Ctrl Pts',(10.7450782430497,-0.325766720886662,
-40.6422852991148));
#15054=CARTESIAN_POINT('Ctrl Pts',(10.7444969181079,-0.343927986990267,
-40.6457102653304));
#15055=CARTESIAN_POINT('Ctrl Pts',(10.7431102516456,-0.387249057198522,
-40.6538800262404));
#15056=CARTESIAN_POINT('Ctrl Pts',(10.7414636104447,-0.430474944517902,
-40.6635775017438));
#15057=CARTESIAN_POINT('Ctrl Pts',(10.7395706012187,-0.473417805392778,
-40.6747168887078));
#15058=CARTESIAN_POINT('Ctrl Pts',(10.7380019900666,-0.509001705115955,
-40.6839473596321));
#15059=CARTESIAN_POINT('Ctrl Pts',(10.7362643862015,-0.544391317906246,
-40.6941668777214));
#15060=CARTESIAN_POINT('Ctrl Pts',(10.7343701126333,-0.579481048012099,
-40.7052999616701));
#15061=CARTESIAN_POINT('Ctrl Pts',(10.7325718074294,-0.612793049673637,
-40.715869017342));
#15062=CARTESIAN_POINT('Ctrl Pts',(10.7306324527749,-0.645834797347597,
-40.727261544876));
#15063=CARTESIAN_POINT('Ctrl Pts',(10.7285656648372,-0.678516863957403,
-40.7393930149516));
#15064=CARTESIAN_POINT('Ctrl Pts',(10.7249857341197,-0.735126219971907,
-40.7604062120877));
#15065=CARTESIAN_POINT('Ctrl Pts',(10.7210297007888,-0.790581697174948,
-40.7836007783321));
#15066=CARTESIAN_POINT('Ctrl Pts',(10.7167394974661,-0.844993427083508,
-40.8087109236785));
#15067=CARTESIAN_POINT('Ctrl Pts',(10.7123146364162,-0.901112992104639,
-40.8346092076849));
#15068=CARTESIAN_POINT('Ctrl Pts',(10.7075342933432,-0.956122257581554,
-40.8625453016496));
#15069=CARTESIAN_POINT('Ctrl Pts',(10.7024356672764,-1.01013949976628,-40.8922833787714));
#15070=CARTESIAN_POINT('Ctrl Pts',(10.6978560693835,-1.05865791340333,-40.918994189398));
#15071=CARTESIAN_POINT('Ctrl Pts',(10.6930195520167,-1.10637595385721,-40.9471596883995));
#15072=CARTESIAN_POINT('Ctrl Pts',(10.6879474115916,-1.15337770355406,-40.9766442613547));
#15073=CARTESIAN_POINT('Ctrl Pts',(10.6831241063421,-1.1980735847896,-41.0046823446087));
#15074=CARTESIAN_POINT('Ctrl Pts',(10.6780884706721,-1.24212147909129,-41.0339143291386));
#15075=CARTESIAN_POINT('Ctrl Pts',(10.6728535582484,-1.28559258333327,-41.0642464718845));
#15076=CARTESIAN_POINT('Ctrl Pts',(10.6660476352044,-1.34210947724856,-41.1036813683216));
#15077=CARTESIAN_POINT('Ctrl Pts',(10.658945115275,-1.39731842014561,-41.1447431707096));
#15078=CARTESIAN_POINT('Ctrl Pts',(10.6515892046568,-1.45131987859543,-41.1871531562581));
#15079=CARTESIAN_POINT('Ctrl Pts',(10.6440807744717,-1.50644101881918,-41.2304424826469));
#15080=CARTESIAN_POINT('Ctrl Pts',(10.6363083207675,-1.56030407412022,-41.275136692109));
#15081=CARTESIAN_POINT('Ctrl Pts',(10.6283098169498,-1.61301335515717,-41.3209937151806));
#15082=CARTESIAN_POINT('Ctrl Pts',(10.6200706514067,-1.66730857111461,-41.3682305000857));
#15083=CARTESIAN_POINT('Ctrl Pts',(10.6115916232549,-1.72037953278926,-41.416701263838));
#15084=CARTESIAN_POINT('Ctrl Pts',(10.6029060066273,-1.77233769176879,-41.466195898445));
#15085=CARTESIAN_POINT('Ctrl Pts',(10.6005973086165,-1.78614853599859,-41.4793519205634));
#15086=CARTESIAN_POINT('Ctrl Pts',(10.5982739708202,-1.79988074355578,-41.4925805664047));
#15087=CARTESIAN_POINT('Ctrl Pts',(10.5959365250946,-1.81353637906657,-41.5058784916094));
#15088=CARTESIAN_POINT('Ctrl Pts',(10.5866048558053,-1.8680530992313,-41.5589671425614));
#15089=CARTESIAN_POINT('Ctrl Pts',(10.5770362062685,-1.92142430401211,-41.6132278236985));
#15090=CARTESIAN_POINT('Ctrl Pts',(10.5672567498948,-1.97377158735742,-41.6684916149444));
#15091=CARTESIAN_POINT('Ctrl Pts',(10.5571324670662,-2.02796465102488,-41.7257040234229));
#15092=CARTESIAN_POINT('Ctrl Pts',(10.5467822523826,-2.08106030959691,-41.7839916348728));
#15093=CARTESIAN_POINT('Ctrl Pts',(10.5362259798091,-2.13319086452431,-41.8432233948788));
#15094=CARTESIAN_POINT('Ctrl Pts',(10.5263487812712,-2.18196791507197,-41.8986448373681));
#15095=CARTESIAN_POINT('Ctrl Pts',(10.5162910689449,-2.22990000148053,-41.9548936385444));
#15096=CARTESIAN_POINT('Ctrl Pts',(10.50606228588,-2.27709359605839,-42.0119030751991));
#15097=CARTESIAN_POINT('Ctrl Pts',(10.5060622858799,-2.27709359605899,-42.0119030751999));
#15098=CARTESIAN_POINT('Ctrl Pts',(10.490385853827,-2.3494215723234,-42.0992746181432));
#15099=CARTESIAN_POINT('Ctrl Pts',(10.4736968030171,-2.42282523877563,-42.1850875945437));
#15100=CARTESIAN_POINT('Ctrl Pts',(10.4558750724626,-2.49744213414836,-42.2692654755833));
#15101=CARTESIAN_POINT('Ctrl Pts',(10.4383088491055,-2.57098925945792,-42.3522365122926));
#15102=CARTESIAN_POINT('Ctrl Pts',(10.4196422455777,-2.64571509969582,-42.4336189546246));
#15103=CARTESIAN_POINT('Ctrl Pts',(10.3997435370924,-2.72174811639428,-42.5132910671944));
#15104=CARTESIAN_POINT('Ctrl Pts',(10.3794106775262,-2.79944002549812,-42.5947014701569));
#15105=CARTESIAN_POINT('Ctrl Pts',(10.3577915447461,-2.87849682700923,-42.6743263557515));
#15106=CARTESIAN_POINT('Ctrl Pts',(10.3347260481738,-2.95905154512446,-42.7519828652624));
#15107=CARTESIAN_POINT('Ctrl Pts',(10.3116605516015,-3.0396062632397,-42.8296393747733));
#15108=CARTESIAN_POINT('Ctrl Pts',(10.2871488217403,-3.12165894470907,-42.9053275688886));
#15109=CARTESIAN_POINT('Ctrl Pts',(10.2610091614508,-3.20533788993066,-42.978810037564));
#15110=CARTESIAN_POINT('Ctrl Pts',(10.2369004525664,-3.28251530186928,-43.0465832000986));
#15111=CARTESIAN_POINT('Ctrl Pts',(10.2114051900379,-3.36107882835082,-43.1124719480028));
#15112=CARTESIAN_POINT('Ctrl Pts',(10.1843579213735,-3.44112785944755,-43.1762137875122));
#15113=CARTESIAN_POINT('Ctrl Pts',(10.181433339465,-3.44978344500928,-43.1831061001133));
#15114=CARTESIAN_POINT('Ctrl Pts',(10.1784905933372,-3.45845639526026,-43.1899732648885));
#15115=CARTESIAN_POINT('Ctrl Pts',(10.1755294601893,-3.46714683325529,-43.1968149158648));
#15116=CARTESIAN_POINT('Ctrl Pts',(10.1534379069397,-3.53198190285161,-43.2478570977958));
#15117=CARTESIAN_POINT('Ctrl Pts',(10.1302922806719,-3.59787987795324,-43.2975482341483));
#15118=CARTESIAN_POINT('Ctrl Pts',(10.1060391066297,-3.66476105295717,-43.3456209213258));
#15119=CARTESIAN_POINT('Ctrl Pts',(10.0774789910471,-3.7435191604564,-43.4022304809556));
#15120=CARTESIAN_POINT('Ctrl Pts',(10.047380801416,-3.82362678339096,-43.4565636983405));
#15121=CARTESIAN_POINT('Ctrl Pts',(10.0157618677699,-3.90473120949845,-43.5081008020532));
#15122=CARTESIAN_POINT('Ctrl Pts',(9.98816221636101,-3.97552594006497,-43.5530866992061));
#15123=CARTESIAN_POINT('Ctrl Pts',(9.95940424480961,-4.04707940129396,-43.5959421869557));
#15124=CARTESIAN_POINT('Ctrl Pts',(9.92951515284022,-4.1191296203893,-43.6363292172926));
#15125=CARTESIAN_POINT('Ctrl Pts',(9.92514363536094,-4.12966753811807,-43.6422361417731));
#15126=CARTESIAN_POINT('Ctrl Pts',(9.92074740166525,-4.14021801800802,-43.6480926845481));
#15127=CARTESIAN_POINT('Ctrl Pts',(9.91632635362652,-4.15078073859809,-43.653898081324));
#15128=CARTESIAN_POINT('Ctrl Pts',(9.8823854072034,-4.23187208401886,-43.6984668485503));
#15129=CARTESIAN_POINT('Ctrl Pts',(9.8469257129122,-4.31382280718569,-43.7400429325073));
#15130=CARTESIAN_POINT('Ctrl Pts',(9.80979522521179,-4.39669658017479,-43.7783856209309));
#15131=CARTESIAN_POINT('Ctrl Pts',(9.79294577200484,-4.43430389013879,-43.7957851590042));
#15132=CARTESIAN_POINT('Ctrl Pts',(9.77575204596624,-4.47210120717099,-43.8125181941916));
#15133=CARTESIAN_POINT('Ctrl Pts',(9.75819873711376,-4.51009410634067,-43.8285588699776));
#15134=CARTESIAN_POINT('Ctrl Pts',(9.73442906213901,-4.56154189161018,-43.8502802247951));
#15135=CARTESIAN_POINT('Ctrl Pts',(9.70992373941314,-4.61351031125972,-43.8707967158323));
#15136=CARTESIAN_POINT('Ctrl Pts',(9.68475440784897,-4.6657702690997,-43.8899311961881));
#15137=CARTESIAN_POINT('Ctrl Pts',(9.65977375932576,-4.71763845778443,-43.90892223404));
#15138=CARTESIAN_POINT('Ctrl Pts',(9.63413899471342,-4.76979381627444,-43.9265518693464));
#15139=CARTESIAN_POINT('Ctrl Pts',(9.60793275939673,-4.82201931450148,-43.9426963378945));
#15140=CARTESIAN_POINT('Ctrl Pts',(9.59807555104078,-4.8416634034481,-43.9487689152163));
#15141=CARTESIAN_POINT('Ctrl Pts',(9.58813762048602,-4.8613174875905,-43.9546318746589));
#15142=CARTESIAN_POINT('Ctrl Pts',(9.57812384114847,-4.88097027922755,-43.9602804639433));
#15143=CARTESIAN_POINT('Ctrl Pts',(9.47988016989897,-5.07378083912112,-44.0156979172321));
#15144=CARTESIAN_POINT('Ctrl Pts',(9.37498500850867,-5.26520200497458,-44.0501809838329));
#15145=CARTESIAN_POINT('Ctrl Pts',(9.2631046846633,-5.45512072416129,-44.0630753329145));
#15146=CARTESIAN_POINT('Ctrl Pts',(9.23044829970098,-5.51055548330521,-44.0668390226589));
#15147=CARTESIAN_POINT('Ctrl Pts',(9.1971967976106,-5.56586196042964,-44.0687635893465));
#15148=CARTESIAN_POINT('Ctrl Pts',(9.16334192291174,-5.6210366840491,-44.0688332970512));
#15149=CARTESIAN_POINT('Ctrl Pts',(9.13431980327446,-5.66833526199634,-44.0688930540393));
#15150=CARTESIAN_POINT('Ctrl Pts',(9.10476428938674,-5.71568116575118,-44.0675714534323));
#15151=CARTESIAN_POINT('Ctrl Pts',(9.07480312871612,-5.76285537335169,-44.0648683451569));
#15152=CARTESIAN_POINT('Ctrl Pts',(9.05948004307397,-5.78698175587437,-44.0634858900492));
#15153=CARTESIAN_POINT('Ctrl Pts',(9.04405107690922,-5.81106335134459,-44.0617428892334));
#15154=CARTESIAN_POINT('Ctrl Pts',(9.02853471299363,-5.83507163077697,-44.0596443418483));
#15155=CARTESIAN_POINT('Ctrl Pts',(8.9982064294724,-5.88199821160759,-44.055542521317));
#15156=CARTESIAN_POINT('Ctrl Pts',(8.96754046580988,-5.92864274808812,-44.0500576047013));
#15157=CARTESIAN_POINT('Ctrl Pts',(8.93668327281857,-5.974796952149,-44.043250137711));
#15158=CARTESIAN_POINT('Ctrl Pts',(8.9345094068387,-5.97804848102476,-44.0427705567944));
#15159=CARTESIAN_POINT('Ctrl Pts',(8.93233459747658,-5.98129757948401,-44.0422844323534));
#15160=CARTESIAN_POINT('Ctrl Pts',(8.93015889852956,-5.98454417612983,-44.0417917948209));
#15161=CARTESIAN_POINT('Ctrl Pts',(8.87228268877637,-6.07090755315648,-44.0286870437248));
#15162=CARTESIAN_POINT('Ctrl Pts',(8.81378786331644,-6.15548448285228,-44.010978867558));
#15163=CARTESIAN_POINT('Ctrl Pts',(8.75476238688098,-6.23831993001784,-43.9890041642558));
#15164=CARTESIAN_POINT('Ctrl Pts',(8.73245078970895,-6.26963168284619,-43.9806977386637));
#15165=CARTESIAN_POINT('Ctrl Pts',(8.71004631052358,-6.30071602093377,-43.9717711696754));
#15166=CARTESIAN_POINT('Ctrl Pts',(8.68756771503185,-6.33155719715209,-43.9622493672949));
#15167=CARTESIAN_POINT('Ctrl Pts',(8.63693389296735,-6.40102802460982,-43.9408011746067));
#15168=CARTESIAN_POINT('Ctrl Pts',(8.58568689344058,-6.46958806014974,-43.9162245598352));
#15169=CARTESIAN_POINT('Ctrl Pts',(8.53411477772601,-6.53692068547023,-43.8887772589834));
#15170=CARTESIAN_POINT('Ctrl Pts',(8.50992046471492,-6.56850881386656,-43.8759007543274));
#15171=CARTESIAN_POINT('Ctrl Pts',(8.485654610908,-6.59982718076872,-43.8623930899435));
#15172=CARTESIAN_POINT('Ctrl Pts',(8.46134684828327,-6.63084530909066,-43.8482841546627));
#15173=CARTESIAN_POINT('Ctrl Pts',(8.40630859602086,-6.70107734145193,-43.8163383457814));
#15174=CARTESIAN_POINT('Ctrl Pts',(8.3511331781303,-6.76968547698108,-43.7813828521671));
#15175=CARTESIAN_POINT('Ctrl Pts',(8.29600947438739,-6.83657937909929,-43.7437667180354));
#15176=CARTESIAN_POINT('Ctrl Pts',(8.25940112988745,-6.88100446027871,-43.718785370565));
#15177=CARTESIAN_POINT('Ctrl Pts',(8.22281581705429,-6.92467378385051,-43.6926316589223));
#15178=CARTESIAN_POINT('Ctrl Pts',(8.18631127030164,-6.96756410281864,-43.6654197758277));
#15179=CARTESIAN_POINT('Ctrl Pts',(8.12642898534381,-7.03792164813442,-43.6207812339839));
#15180=CARTESIAN_POINT('Ctrl Pts',(8.06676026536889,-7.10619090896531,-43.5733019776517));
#15181=CARTESIAN_POINT('Ctrl Pts',(8.00730071472223,-7.17256758947659,-43.5232728467731));
#15182=CARTESIAN_POINT('Ctrl Pts',(7.94784116407556,-7.23894426998787,-43.4732437158945));
#15183=CARTESIAN_POINT('Ctrl Pts',(7.88859071459035,-7.30342827304296,-43.4206643974407));
#15184=CARTESIAN_POINT('Ctrl Pts',(7.82953376242443,-7.3661999065718,-43.3657719705771));
#15185=CARTESIAN_POINT('Ctrl Pts',(7.78246051217696,-7.4162340635199,-43.3220181896644));
#15186=CARTESIAN_POINT('Ctrl Pts',(7.73551173823827,-7.46518289020138,-43.2768135657487));
#15187=CARTESIAN_POINT('Ctrl Pts',(7.68867196096467,-7.51312673470191,-43.2302274255216));
#15188=CARTESIAN_POINT('Ctrl Pts',(7.62941400079359,-7.57378147290157,-43.1712903467654));
#15189=CARTESIAN_POINT('Ctrl Pts',(7.57024340356674,-7.63291386982353,-43.1100539400161));
#15190=CARTESIAN_POINT('Ctrl Pts',(7.51134952905245,-7.69045086723973,-43.0468902512232));
#15191=CARTESIAN_POINT('Ctrl Pts',(7.4510109776655,-7.74939925709996,-42.9821771462789));
#15192=CARTESIAN_POINT('Ctrl Pts',(7.39096291968201,-7.80667305865563,-42.9154410886981));
#15193=CARTESIAN_POINT('Ctrl Pts',(7.33141801277851,-7.86220712602253,-42.8471352398619));
#15194=CARTESIAN_POINT('Ctrl Pts',(7.28787285714568,-7.90281915704535,-42.7971832125118));
#15195=CARTESIAN_POINT('Ctrl Pts',(7.24459698063875,-7.9425010699813,-42.746392803258));
#15196=CARTESIAN_POINT('Ctrl Pts',(7.20167632415019,-7.98123150622032,-42.6949580898006));
#15197=CARTESIAN_POINT('Ctrl Pts',(7.13930068925887,-8.03751758727477,-42.6202091653936));
#15198=CARTESIAN_POINT('Ctrl Pts',(7.07752996222588,-8.0919282722449,-42.543925714373));
#15199=CARTESIAN_POINT('Ctrl Pts',(7.01632524916812,-8.14464761366221,-42.4662769769472));
#15200=CARTESIAN_POINT('Ctrl Pts',(6.95400229919708,-8.19833016053661,-42.3872095630809));
#15201=CARTESIAN_POINT('Ctrl Pts',(6.89226620642754,-8.25025895328182,-42.3067264627181));
#15202=CARTESIAN_POINT('Ctrl Pts',(6.83106473230173,-8.30061305883954,-42.2249555226949));
#15203=CARTESIAN_POINT('Ctrl Pts',(6.79926069456621,-8.32678013890045,-42.1824623295273));
#15204=CARTESIAN_POINT('Ctrl Pts',(6.76760085014226,-8.35252173355581,-42.13962053505));
#15205=CARTESIAN_POINT('Ctrl Pts',(6.73607674834671,-8.37786144795066,-42.0964428903655));
#15206=CARTESIAN_POINT('Ctrl Pts',(6.67199336517915,-8.42937297514509,-42.0086697456609));
#15207=CARTESIAN_POINT('Ctrl Pts',(6.60851060516834,-8.4791932576748,-41.9195563684189));
#15208=CARTESIAN_POINT('Ctrl Pts',(6.54557135950043,-8.52749545016914,-41.8292245834684));
#15209=CARTESIAN_POINT('Ctrl Pts',(6.49978585112311,-8.56263315186264,-41.7635122182708));
#15210=CARTESIAN_POINT('Ctrl Pts',(6.45428772304682,-8.59696718414578,-41.697154000995));
#15211=CARTESIAN_POINT('Ctrl Pts',(6.40905142763883,-8.63055964574283,-41.6301805545864));
#15212=CARTESIAN_POINT('Ctrl Pts',(6.35304742575302,-8.67214820346318,-41.5472652542699));
#15213=CARTESIAN_POINT('Ctrl Pts',(6.29738512281016,-8.71263450139334,-41.4632867952234));
#15214=CARTESIAN_POINT('Ctrl Pts',(6.24209165749993,-8.75206999235691,-41.3783888763224));
#15215=CARTESIAN_POINT('Ctrl Pts',(6.18469411014494,-8.79300612192211,-41.2902603372063));
#15216=CARTESIAN_POINT('Ctrl Pts',(6.12769384919897,-8.83281008866344,-41.2011409070487));
#15217=CARTESIAN_POINT('Ctrl Pts',(6.07110079616866,-8.87154004941081,-41.1111391356439));
#15218=CARTESIAN_POINT('Ctrl Pts',(6.05484968674209,-8.88266164113435,-41.0852944681915));
#15219=CARTESIAN_POINT('Ctrl Pts',(6.03863203907221,-8.89369466738167,-41.0593767317759));
#15220=CARTESIAN_POINT('Ctrl Pts',(6.02244782123643,-8.90464048912061,-41.0333877658766));
#15221=CARTESIAN_POINT('Ctrl Pts',(5.96789208360707,-8.94153800156061,-40.9457809862815));
#15222=CARTESIAN_POINT('Ctrl Pts',(5.91381192380562,-8.97738468492097,-40.8575269837696));
#15223=CARTESIAN_POINT('Ctrl Pts',(5.86012825013986,-9.01229190082115,-40.7685826949035));
#15224=CARTESIAN_POINT('Ctrl Pts',(5.78173848263364,-9.0632639813785,-40.638704807473));
#15225=CARTESIAN_POINT('Ctrl Pts',(5.70446841167932,-9.11205487886131,-40.5078066310375));
#15226=CARTESIAN_POINT('Ctrl Pts',(5.62824515844197,-9.15889493533431,-40.3760464765655));
#15227=CARTESIAN_POINT('Ctrl Pts',(5.55068166324207,-9.20655858574416,-40.2419695686026));
#15228=CARTESIAN_POINT('Ctrl Pts',(5.47420216133207,-9.25220373228151,-40.107007556575));
#15229=CARTESIAN_POINT('Ctrl Pts',(5.39872201476634,-9.29604069692326,-39.9712454669586));
#15230=CARTESIAN_POINT('Ctrl Pts',(5.32192875426745,-9.34064028500545,-39.833121549768));
#15231=CARTESIAN_POINT('Ctrl Pts',(5.24616988281148,-9.3833681445475,-39.6941694464635));
#15232=CARTESIAN_POINT('Ctrl Pts',(5.17134976653292,-9.42442267008781,-39.5544301786707));
#15233=CARTESIAN_POINT('Ctrl Pts',(5.13294490286178,-9.44549579232929,-39.4827025765763));
#15234=CARTESIAN_POINT('Ctrl Pts',(5.09478727515637,-9.4661276745041,-39.4107668026536));
#15235=CARTESIAN_POINT('Ctrl Pts',(5.05686335325628,-9.48634295751582,-39.3386236125273));
#15236=CARTESIAN_POINT('Ctrl Pts',(4.97902793754603,-9.52783299541494,-39.1905562473182));
#15237=CARTESIAN_POINT('Ctrl Pts',(4.90219178004977,-9.56756126829831,-39.0416213059113));
#15238=CARTESIAN_POINT('Ctrl Pts',(4.82630358622877,-9.60569069322725,-38.8919330766794));
#15239=CARTESIAN_POINT('Ctrl Pts',(4.73610193406239,-9.65101180250094,-38.7140117834354));
#15240=CARTESIAN_POINT('Ctrl Pts',(4.64723779780822,-9.6940793596263,-38.5350724280117));
#15241=CARTESIAN_POINT('Ctrl Pts',(4.55961797968078,-9.73512502144953,-38.3551653870197));
#15242=CARTESIAN_POINT('Ctrl Pts',(4.47869953974762,-9.77303141057178,-38.1890180769569));
#15243=CARTESIAN_POINT('Ctrl Pts',(4.39884221209784,-9.80921297956952,-38.0220450111243));
#15244=CARTESIAN_POINT('Ctrl Pts',(4.31996655994152,-9.84383312150245,-37.854251824959));
#15245=CARTESIAN_POINT('Ctrl Pts',(4.21884999459777,-9.88821525652471,-37.6391452589999));
#15246=CARTESIAN_POINT('Ctrl Pts',(4.11934342920933,-9.93003289724673,-37.422735917508));
#15247=CARTESIAN_POINT('Ctrl Pts',(4.02137300417622,-9.96955084295716,-37.205166603912));
#15248=CARTESIAN_POINT('Ctrl Pts',(3.92418102114997,-10.0087547915715,-36.9893260272593));
#15249=CARTESIAN_POINT('Ctrl Pts',(3.82850078243586,-10.0456952251983,-36.772343879366));
#15250=CARTESIAN_POINT('Ctrl Pts',(3.73425145285707,-10.0806028780048,-36.55431574799));
#15251=CARTESIAN_POINT('Ctrl Pts',(3.63886981326191,-10.1159299108228,-36.3336682299498));
#15252=CARTESIAN_POINT('Ctrl Pts',(3.54495362444972,-10.1491749110926,-36.1119496058682));
#15253=CARTESIAN_POINT('Ctrl Pts',(3.4524110597738,-10.1805508308637,-35.889212141429));
#15254=CARTESIAN_POINT('Ctrl Pts',(3.35986849509789,-10.2119267506348,-35.6664746769898));
#15255=CARTESIAN_POINT('Ctrl Pts',(3.26869949929918,-10.2414334400909,-35.4427184156961));
#15256=CARTESIAN_POINT('Ctrl Pts',(3.17880504329623,-10.2692598806778,-35.2179476947513));
#15257=CARTESIAN_POINT('Ctrl Pts',(3.11875845584299,-10.287847042473,-35.0678081271711));
#15258=CARTESIAN_POINT('Ctrl Pts',(3.05925105749683,-10.3056863347943,-34.9170987408754));
#15259=CARTESIAN_POINT('Ctrl Pts',(3.00037766351643,-10.322797517479,-34.766133239422));
#15260=CARTESIAN_POINT('Ctrl Pts',(2.93300394147518,-10.3423792671974,-34.5933708582329));
#15261=CARTESIAN_POINT('Ctrl Pts',(2.86626401996985,-10.3610642855586,-34.4197841786842));
#15262=CARTESIAN_POINT('Ctrl Pts',(2.80032934335272,-10.3788556834136,-34.245878496818));
#15263=CARTESIAN_POINT('Ctrl Pts',(2.78727949802178,-10.3823769714845,-34.2114589414799));
#15264=CARTESIAN_POINT('Ctrl Pts',(2.77426113538516,-10.3858632617225,-34.1770267382144));
#15265=CARTESIAN_POINT('Ctrl Pts',(2.76127549569092,-10.3893145893703,-34.142585582622));
#15266=CARTESIAN_POINT('Ctrl Pts',(2.6314416790793,-10.4238218644405,-33.7982339153683));
#15267=CARTESIAN_POINT('Ctrl Pts',(2.50457200205134,-10.4549409999092,-33.4522457830409));
#15268=CARTESIAN_POINT('Ctrl Pts',(2.38057046060466,-10.4830999541101,-33.1049548942437));
#15269=CARTESIAN_POINT('Ctrl Pts',(2.36970090201688,-10.4855682734462,-33.0745125415217));
#15270=CARTESIAN_POINT('Ctrl Pts',(2.35885337811822,-10.4880138159899,-33.0440601702302));
#15271=CARTESIAN_POINT('Ctrl Pts',(2.34802782249378,-10.4904368519569,-33.0135979999854));
#15272=CARTESIAN_POINT('Ctrl Pts',(2.21770246909838,-10.5196069961643,-32.6468738114017));
#15273=CARTESIAN_POINT('Ctrl Pts',(2.09055855130271,-10.5455214163713,-32.2787518271881));
#15274=CARTESIAN_POINT('Ctrl Pts',(1.96649166390134,-10.5686065331557,-31.9094939634275));
#15275=CARTESIAN_POINT('Ctrl Pts',(1.9280261851357,-10.5757638020135,-31.7950099071654));
#15276=CARTESIAN_POINT('Ctrl Pts',(1.88985642821586,-10.5826487298252,-31.680416686595));
#15277=CARTESIAN_POINT('Ctrl Pts',(1.85197914734771,-10.5892730327154,-31.5657221242989));
#15278=CARTESIAN_POINT('Ctrl Pts',(1.74502317759947,-10.6079784076336,-31.2418533603839));
#15279=CARTESIAN_POINT('Ctrl Pts',(1.6403504494956,-10.6246161413583,-30.9170110061736));
#15280=CARTESIAN_POINT('Ctrl Pts',(1.53788875472694,-10.6394265906664,-30.5913659316435));
#15281=CARTESIAN_POINT('Ctrl Pts',(1.41260154985877,-10.6575363808746,-30.1931765277));
#15282=CARTESIAN_POINT('Ctrl Pts',(1.29061928908997,-10.6729130832063,-29.7937918413145));
#15283=CARTESIAN_POINT('Ctrl Pts',(1.17182931764376,-10.6859396294529,-29.3933438455856));
#15284=CARTESIAN_POINT('Ctrl Pts',(1.06436790256251,-10.6977238825867,-29.0310850811159));
#15285=CARTESIAN_POINT('Ctrl Pts',(0.959518682671932,-10.7075839906054,
-28.6679570013368));
#15286=CARTESIAN_POINT('Ctrl Pts',(0.85719280919927,-10.7157695937709,-28.3040700635745));
#15287=CARTESIAN_POINT('Ctrl Pts',(0.822247336604926,-10.7185650721908,
-28.1797984538686));
#15288=CARTESIAN_POINT('Ctrl Pts',(0.787596463964595,-10.7211649655967,
-28.0554372461487));
#15289=CARTESIAN_POINT('Ctrl Pts',(0.753236825127353,-10.7235784272451,
-27.9309927285396));
#15290=CARTESIAN_POINT('Ctrl Pts',(0.636205486739294,-10.7317988467963,
-27.5071259783727));
#15291=CARTESIAN_POINT('Ctrl Pts',(0.52256763618542,-10.7378574576103,-27.08220648135));
#15292=CARTESIAN_POINT('Ctrl Pts',(0.412205680126688,-10.7420921052949,
-26.6564401459235));
#15293=CARTESIAN_POINT('Ctrl Pts',(0.334985882992854,-10.7450550704943,
-26.3585332292451));
#15294=CARTESIAN_POINT('Ctrl Pts',(0.259459073243975,-10.7471216958854,
-26.060554842328));
#15295=CARTESIAN_POINT('Ctrl Pts',(0.185425494016263,-10.7483995046789,
-25.7619706453529));
#15296=CARTESIAN_POINT('Ctrl Pts',(0.122586226530908,-10.7494841012823,
-25.5085341315934));
#15297=CARTESIAN_POINT('Ctrl Pts',(0.0608224917771859,-10.75,-25.2546607217708));
#15298=CARTESIAN_POINT('Ctrl Pts',(2.5146574731546E-15,-10.75,-25.));
#15299=CARTESIAN_POINT('',(-10.5060622858798,-2.27709359605911,-42.0119030752));
#15300=CARTESIAN_POINT('Ctrl Pts',(2.37847882546591E-15,-10.75,-25.));
#15301=CARTESIAN_POINT('Ctrl Pts',(-0.107236928456273,-10.75,-25.4489956397202));
#15302=CARTESIAN_POINT('Ctrl Pts',(-0.217860528274796,-10.7483974074849,
-25.8972288329737));
#15303=CARTESIAN_POINT('Ctrl Pts',(-0.332035266389469,-10.7448689509013,
-26.3445236238487));
#15304=CARTESIAN_POINT('Ctrl Pts',(-0.441369847169077,-10.7414900745602,
-26.7728564516946));
#15305=CARTESIAN_POINT('Ctrl Pts',(-0.553961059582523,-10.7363452340984,
-27.2003277499857));
#15306=CARTESIAN_POINT('Ctrl Pts',(-0.669944683009056,-10.7291037616657,
-27.6267852425981));
#15307=CARTESIAN_POINT('Ctrl Pts',(-0.697532936495075,-10.7273812807569,
-27.7282238514259));
#15308=CARTESIAN_POINT('Ctrl Pts',(-0.725313081771794,-10.7255399552348,
-27.8296051483714));
#15309=CARTESIAN_POINT('Ctrl Pts',(-0.753286850688558,-10.7235749134903,
-27.9309272016471));
#15310=CARTESIAN_POINT('Ctrl Pts',(-0.867733545662818,-10.7155355057934,
-28.3454574767741));
#15311=CARTESIAN_POINT('Ctrl Pts',(-0.985408417919781,-10.7054316754645,
-28.7590760985836));
#15312=CARTESIAN_POINT('Ctrl Pts',(-1.10644537552961,-10.6929073769954,
-29.1716055677841));
#15313=CARTESIAN_POINT('Ctrl Pts',(-1.22118601148511,-10.681034590372,-29.5626753251639));
#15314=CARTESIAN_POINT('Ctrl Pts',(-1.33894815018126,-10.6669865555435,
-29.9527656100601));
#15315=CARTESIAN_POINT('Ctrl Pts',(-1.45983743148625,-10.6504165883258,
-30.3417420844204));
#15316=CARTESIAN_POINT('Ctrl Pts',(-1.48571264619969,-10.6468699425444,
-30.4249988436955));
#15317=CARTESIAN_POINT('Ctrl Pts',(-1.51173109023162,-10.6432075943637,
-30.5082046613194));
#15318=CARTESIAN_POINT('Ctrl Pts',(-1.53789373804128,-10.6394258703545,
-30.5913583746477));
#15319=CARTESIAN_POINT('Ctrl Pts',(-1.64034562245505,-10.6246167901002,
-30.9169849965578));
#15320=CARTESIAN_POINT('Ctrl Pts',(-1.74501002042912,-10.6079804855205,
-31.2418078298158));
#15321=CARTESIAN_POINT('Ctrl Pts',(-1.85195771748882,-10.5892767805307,
-31.5656535771436));
#15322=CARTESIAN_POINT('Ctrl Pts',(-1.97412810450694,-10.5679108330621,
-31.9355947855375));
#15323=CARTESIAN_POINT('Ctrl Pts',(-2.09934183067117,-10.5438372894304,
-32.3044816612346));
#15324=CARTESIAN_POINT('Ctrl Pts',(-2.2277055130733,-10.5166457094765,-32.6720516062204));
#15325=CARTESIAN_POINT('Ctrl Pts',(-2.26750916245566,-10.5082140090579,
-32.7860295238053));
#15326=CARTESIAN_POINT('Ctrl Pts',(-2.30761563823564,-10.4994821320271,
-32.8998808229037));
#15327=CARTESIAN_POINT('Ctrl Pts',(-2.34802797257565,-10.490436818365,-33.0135977355672));
#15328=CARTESIAN_POINT('Ctrl Pts',(-2.47153733442923,-10.4627922653735,
-33.361142700351));
#15329=CARTESIAN_POINT('Ctrl Pts',(-2.59790667502491,-10.4322221869952,
-33.7074132250065));
#15330=CARTESIAN_POINT('Ctrl Pts',(-2.72723242795073,-10.3983029233844,
-34.0520766841272));
#15331=CARTESIAN_POINT('Ctrl Pts',(-2.73855743066555,-10.3953326274937,
-34.0822587207435));
#15332=CARTESIAN_POINT('Ctrl Pts',(-2.7499051011573,-10.3923366166284,-34.1124284254007));
#15333=CARTESIAN_POINT('Ctrl Pts',(-2.76127550222569,-10.3893145876335,
-34.1425855701607));
#15334=CARTESIAN_POINT('Ctrl Pts',(-2.82688668944206,-10.3718764243739,
-34.3166028329513));
#15335=CARTESIAN_POINT('Ctrl Pts',(-2.89333478271947,-10.3535455195258,
-34.4903953522009));
#15336=CARTESIAN_POINT('Ctrl Pts',(-2.96045216143973,-10.3343182819924,
-34.6634673794312));
#15337=CARTESIAN_POINT('Ctrl Pts',(-2.97372789205513,-10.3305151593014,
-34.6977008023446));
#15338=CARTESIAN_POINT('Ctrl Pts',(-2.98702974736202,-10.3266769758128,
-34.7319058852893));
#15339=CARTESIAN_POINT('Ctrl Pts',(-3.0003563392787,-10.3228037152111,-34.7660785653851));
#15340=CARTESIAN_POINT('Ctrl Pts',(-3.05923669243037,-10.3056906413286,
-34.9170623641507));
#15341=CARTESIAN_POINT('Ctrl Pts',(-3.11875120968947,-10.2878492854881,
-35.0677900111587));
#15342=CARTESIAN_POINT('Ctrl Pts',(-3.17880504322316,-10.2692598807004,
-35.2179476948946));
#15343=CARTESIAN_POINT('Ctrl Pts',(-3.2683423400296,-10.2415439972009,-35.441825377722));
#15344=CARTESIAN_POINT('Ctrl Pts',(-3.35914405717459,-10.2121611770437,
-35.6646965966392));
#15345=CARTESIAN_POINT('Ctrl Pts',(-3.45130806413639,-10.1809247273861,
-35.8865571686432));
#15346=CARTESIAN_POINT('Ctrl Pts',(-3.54283782722993,-10.1499032372048,
-36.1068909655857));
#15347=CARTESIAN_POINT('Ctrl Pts',(-3.63571123979394,-10.1170536586038,
-36.3262278829965));
#15348=CARTESIAN_POINT('Ctrl Pts',(-3.73001725013496,-10.0821701109077,
-36.544517773388));
#15349=CARTESIAN_POINT('Ctrl Pts',(-3.82530348275741,-10.0469239815418,
-36.7650765818855));
#15350=CARTESIAN_POINT('Ctrl Pts',(-3.92205232525191,-10.0096015921242,
-36.9845664962694));
#15351=CARTESIAN_POINT('Ctrl Pts',(-4.02034750444548,-9.96996443329666,
-37.2028890356457));
#15352=CARTESIAN_POINT('Ctrl Pts',(-4.11864268363905,-9.93032727446916,
-37.4212115750219));
#15353=CARTESIAN_POINT('Ctrl Pts',(-4.21848427270404,-9.88837553748256,
-37.6383666359865));
#15354=CARTESIAN_POINT('Ctrl Pts',(-4.31994691208665,-9.84384174532468,
-37.8542100277663));
#15355=CARTESIAN_POINT('Ctrl Pts',(-4.40535485324238,-9.80635465132431,
-38.0358999563563));
#15356=CARTESIAN_POINT('Ctrl Pts',(-4.49191389414606,-9.76703709859576,
-38.2166288568363));
#15357=CARTESIAN_POINT('Ctrl Pts',(-4.57972460026303,-9.72568071364687,
-38.3963878422841));
#15358=CARTESIAN_POINT('Ctrl Pts',(-4.660825535451,-9.68748444301353,-38.562411126607));
#15359=CARTESIAN_POINT('Ctrl Pts',(-4.74299414114367,-9.64754886736609,
-38.7276065505638));
#15360=CARTESIAN_POINT('Ctrl Pts',(-4.82630358598209,-9.6056906933512,-38.8919330774143));
#15361=CARTESIAN_POINT('Ctrl Pts',(-4.90218572876413,-9.56756430872154,
-39.0416093715911));
#15362=CARTESIAN_POINT('Ctrl Pts',(-4.97901568325355,-9.52783933124077,
-39.1905324952367));
#15363=CARTESIAN_POINT('Ctrl Pts',(-5.05684473081742,-9.48635288415197,
-39.3385881853712));
#15364=CARTESIAN_POINT('Ctrl Pts',(-5.13087767171036,-9.4468899357886,-39.4794224689669));
#15365=CARTESIAN_POINT('Ctrl Pts',(-5.20580158432899,-9.40584069228541,
-39.6194691944838));
#15366=CARTESIAN_POINT('Ctrl Pts',(-5.28171573037305,-9.36301668773194,
-39.7587113462651));
#15367=CARTESIAN_POINT('Ctrl Pts',(-5.35632406140468,-9.32092930778603,
-39.8955583648382));
#15368=CARTESIAN_POINT('Ctrl Pts',(-5.43188888889226,-9.27712777591539,
-40.03162827474));
#15369=CARTESIAN_POINT('Ctrl Pts',(-5.50849864103087,-9.23141218467567,
-40.1668597120882));
#15370=CARTESIAN_POINT('Ctrl Pts',(-5.54813074290765,-9.20776238920196,
-40.236818248075));
#15371=CARTESIAN_POINT('Ctrl Pts',(-5.5880423937018,-9.18359999174024,-40.306551642029));
#15372=CARTESIAN_POINT('Ctrl Pts',(-5.62824515816366,-9.15889493550534,
-40.3760464775997));
#15373=CARTESIAN_POINT('Ctrl Pts',(-5.70446273045627,-9.11205837004071,
-40.5077968118111));
#15374=CARTESIAN_POINT('Ctrl Pts',(-5.78172696287714,-9.06327125490934,
-40.6386852930282));
#15375=CARTESIAN_POINT('Ctrl Pts',(-5.86011071648358,-9.01230330186323,
-40.7685536452044));
#15376=CARTESIAN_POINT('Ctrl Pts',(-5.91380013799187,-8.9773924971543,-40.8575077508675));
#15377=CARTESIAN_POINT('Ctrl Pts',(-5.96788613468601,-8.94154202497618,
-40.9457714335175));
#15378=CARTESIAN_POINT('Ctrl Pts',(-6.02244782126864,-8.90464048909882,
-41.033387765718));
#15379=CARTESIAN_POINT('Ctrl Pts',(-6.07897394773201,-8.86641034970353,
-41.1241586378155));
#15380=CARTESIAN_POINT('Ctrl Pts',(-6.13590921690286,-8.82711651281615,
-41.2140642892948));
#15381=CARTESIAN_POINT('Ctrl Pts',(-6.19324883006869,-8.78670052801951,
-41.3030092871971));
#15382=CARTESIAN_POINT('Ctrl Pts',(-6.2484433970759,-8.74779648493556,-41.3886268973558));
#15383=CARTESIAN_POINT('Ctrl Pts',(-6.30401276338849,-8.70785255276022,
-41.473354491277));
#15384=CARTESIAN_POINT('Ctrl Pts',(-6.35993531645609,-8.6668165858521,-41.5570616078848));
#15385=CARTESIAN_POINT('Ctrl Pts',(-6.37627760345097,-8.65482461639544,
-41.5815233974147));
#15386=CARTESIAN_POINT('Ctrl Pts',(-6.39264992800991,-8.64273939524507,
-41.6058977286819));
#15387=CARTESIAN_POINT('Ctrl Pts',(-6.40905142809471,-8.63055964540428,
-41.6301805523162));
#15388=CARTESIAN_POINT('Ctrl Pts',(-6.47123616751939,-8.58438127353639,
-41.7222465860561));
#15389=CARTESIAN_POINT('Ctrl Pts',(-6.53391610437926,-8.53680207853486,
-41.8131519097605));
#15390=CARTESIAN_POINT('Ctrl Pts',(-6.59715617551305,-8.48765892208744,
-41.9028104104421));
#15391=CARTESIAN_POINT('Ctrl Pts',(-6.64315450337938,-8.45191413271376,
-41.9680244596425));
#15392=CARTESIAN_POINT('Ctrl Pts',(-6.68944896828638,-8.41534166164106,
-42.032577915456));
#15393=CARTESIAN_POINT('Ctrl Pts',(-6.7360609646428,-8.37787413518879,-42.0964212692318));
#15394=CARTESIAN_POINT('Ctrl Pts',(-6.79685557704122,-8.32900637739579,
-42.1796902182238));
#15395=CARTESIAN_POINT('Ctrl Pts',(-6.85815567166274,-8.27864483482428,
-42.261713048695));
#15396=CARTESIAN_POINT('Ctrl Pts',(-6.92001935262134,-8.22661679423917,
-42.3423866350749));
#15397=CARTESIAN_POINT('Ctrl Pts',(-6.98076429143663,-8.17552962818229,
-42.4216013211836));
#15398=CARTESIAN_POINT('Ctrl Pts',(-7.04205264230787,-8.12283573116821,
-42.4995151701438));
#15399=CARTESIAN_POINT('Ctrl Pts',(-7.10392919618789,-8.06835766777112,
-42.5759835346934));
#15400=CARTESIAN_POINT('Ctrl Pts',(-7.1363436199763,-8.03981898997807,-42.6160419707162));
#15401=CARTESIAN_POINT('Ctrl Pts',(-7.1689192886304,-8.01079045543132,-42.655702938772));
#15402=CARTESIAN_POINT('Ctrl Pts',(-7.20166145050655,-7.98124492776838,
-42.6949402656683));
#15403=CARTESIAN_POINT('Ctrl Pts',(-7.26062011123685,-7.92804243160559,
-42.7655947402625));
#15404=CARTESIAN_POINT('Ctrl Pts',(-7.32024875521799,-7.87304406860132,
-42.8350315342485));
#15405=CARTESIAN_POINT('Ctrl Pts',(-7.38032570970279,-7.81630681975916,
-42.9027542880909));
#15406=CARTESIAN_POINT('Ctrl Pts',(-7.4388878889716,-7.76100013907921,-42.9687694861833));
#15407=CARTESIAN_POINT('Ctrl Pts',(-7.49787602404359,-7.70404110593112,
-43.0331559083555));
#15408=CARTESIAN_POINT('Ctrl Pts',(-7.55709259594321,-7.64549410744107,
-43.0955009361251));
#15409=CARTESIAN_POINT('Ctrl Pts',(-7.6008485065959,-7.60223295346451,-43.1415685043279));
#15410=CARTESIAN_POINT('Ctrl Pts',(-7.64472929780332,-7.55810501353939,
-43.1865224376509));
#15411=CARTESIAN_POINT('Ctrl Pts',(-7.68865828488654,-7.51314073311559,
-43.2302138221607));
#15412=CARTESIAN_POINT('Ctrl Pts',(-7.73550259879265,-7.46519241910727,
-43.276804765109));
#15413=CARTESIAN_POINT('Ctrl Pts',(-7.78245593008502,-7.4162389338257,-43.3220139301321));
#15414=CARTESIAN_POINT('Ctrl Pts',(-7.82953376245117,-7.36619990654337,
-43.3657719702808));
#15415=CARTESIAN_POINT('Ctrl Pts',(-7.88858871032258,-7.30343040337868,
-43.4206625344818));
#15416=CARTESIAN_POINT('Ctrl Pts',(-7.94783714305809,-7.23894864602518,
-43.4732401474993));
#15417=CARTESIAN_POINT('Ctrl Pts',(-8.00729466189739,-7.17257434644111,
-43.5232677541091));
#15418=CARTESIAN_POINT('Ctrl Pts',(-8.06675218073669,-7.10620004685704,
-43.5732953607189));
#15419=CARTESIAN_POINT('Ctrl Pts',(-8.12641885383387,-7.03793330216102,
-43.6207732738916));
#15420=CARTESIAN_POINT('Ctrl Pts',(-8.18629907590924,-6.96757843036117,
-43.6654106856205));
#15421=CARTESIAN_POINT('Ctrl Pts',(-8.24126515827592,-6.90299731251927,
-43.7063848765085));
#15422=CARTESIAN_POINT('Ctrl Pts',(-8.29641393582101,-6.83664939601852,
-43.7449577655475));
#15423=CARTESIAN_POINT('Ctrl Pts',(-8.35154990804721,-6.76861619784635,
-43.7807474993288));
#15424=CARTESIAN_POINT('Ctrl Pts',(-8.38817263164103,-6.72342680675987,
-43.8045199563082));
#15425=CARTESIAN_POINT('Ctrl Pts',(-8.42478989207236,-6.67749412561543,
-43.8270654294201));
#15426=CARTESIAN_POINT('Ctrl Pts',(-8.46134684828446,-6.6308453090891,-43.8482841545959));
#15427=CARTESIAN_POINT('Ctrl Pts',(-8.51315982677914,-6.56472891489431,
-43.878357920717));
#15428=CARTESIAN_POINT('Ctrl Pts',(-8.56478254756177,-6.49724643102362,
-43.9056970712767));
#15429=CARTESIAN_POINT('Ctrl Pts',(-8.61592734856606,-6.42870112309732,
-43.9300233883366));
#15430=CARTESIAN_POINT('Ctrl Pts',(-8.63991916882605,-6.39654679508858,
-43.9414347657402));
#15431=CARTESIAN_POINT('Ctrl Pts',(-8.66380578479096,-6.36415902910658,
-43.9521837717434));
#15432=CARTESIAN_POINT('Ctrl Pts',(-8.68755748755692,-6.33157122947102,
-43.9622450359249));
#15433=CARTESIAN_POINT('Ctrl Pts',(-8.71003951524837,-6.30072544881144,
-43.9717684634522));
#15434=CARTESIAN_POINT('Ctrl Pts',(-8.73244740634611,-6.26963643100528,
-43.9806964803171));
#15435=CARTESIAN_POINT('Ctrl Pts',(-8.75476238684818,-6.23831993006387,
-43.9890041654457));
#15436=CARTESIAN_POINT('Ctrl Pts',(-8.81378476346969,-6.15548883313053,
-44.0109777145809));
#15437=CARTESIAN_POINT('Ctrl Pts',(-8.87227654185961,-6.07091644084465,
-44.0286851829401));
#15438=CARTESIAN_POINT('Ctrl Pts',(-8.93014977420608,-5.98455779150123,
-44.0417897287885));
#15439=CARTESIAN_POINT('Ctrl Pts',(-8.96103257271584,-5.93847436641655,
-44.0487826861988));
#15440=CARTESIAN_POINT('Ctrl Pts',(-8.99173501046696,-5.89188620680568,
-44.0544592798445));
#15441=CARTESIAN_POINT('Ctrl Pts',(-9.02210965563884,-5.84500106362589,
-44.0587554593272));
#15442=CARTESIAN_POINT('Ctrl Pts',(-9.02425298421215,-5.84169270343033,
-44.0590586109916));
#15443=CARTESIAN_POINT('Ctrl Pts',(-9.0263946863895,-5.83838286767396,-44.0593549098961));
#15444=CARTESIAN_POINT('Ctrl Pts',(-9.0285347129843,-5.8350716307914,-44.0596443429015));
#15445=CARTESIAN_POINT('Ctrl Pts',(-9.05887335223018,-5.78812902667531,
-44.0637475645898));
#15446=CARTESIAN_POINT('Ctrl Pts',(-9.08887701333448,-5.74090566264086,
-44.066488459587));
#15447=CARTESIAN_POINT('Ctrl Pts',(-9.11841089904989,-5.69361667178038,
-44.06784174946));
#15448=CARTESIAN_POINT('Ctrl Pts',(-9.1335134748262,-5.66943476850028,-44.0685337736336));
#15449=CARTESIAN_POINT('Ctrl Pts',(-9.14849342989083,-5.64523582718241,
-44.0688637450225));
#15450=CARTESIAN_POINT('Ctrl Pts',(-9.16333413070458,-5.62104938331968,
-44.0688333130625));
#15451=CARTESIAN_POINT('Ctrl Pts',(-9.27932019115726,-5.43202257284732,
-44.0685954750252));
#15452=CARTESIAN_POINT('Ctrl Pts',(-9.38822404812592,-5.24145243072908,
-44.0465840027153));
#15453=CARTESIAN_POINT('Ctrl Pts',(-9.49037895961188,-5.04946426357109,
-44.0034442093763));
#15454=CARTESIAN_POINT('Ctrl Pts',(-9.52019775455593,-4.9934233380307,-43.9908517981765));
#15455=CARTESIAN_POINT('Ctrl Pts',(-9.54944152478437,-4.93726132129649,
-43.9764593736512));
#15456=CARTESIAN_POINT('Ctrl Pts',(-9.57811856097544,-4.88098064194923,
-43.9602834423684));
#15457=CARTESIAN_POINT('Ctrl Pts',(-9.6047301766366,-4.82875349413803,-43.9452725582802));
#15458=CARTESIAN_POINT('Ctrl Pts',(-9.63080521238752,-4.77651667385336,
-43.9287441414904));
#15459=CARTESIAN_POINT('Ctrl Pts',(-9.65625625560094,-4.7244842804683,-43.9108030046276));
#15460=CARTESIAN_POINT('Ctrl Pts',(-9.6818871281723,-4.67208424196093,-43.8927351011291));
#15461=CARTESIAN_POINT('Ctrl Pts',(-9.70688517903262,-4.61989153984246,
-43.8732344536602));
#15462=CARTESIAN_POINT('Ctrl Pts',(-9.73117419853498,-4.56813204941783,
-43.8524589796889));
#15463=CARTESIAN_POINT('Ctrl Pts',(-9.74028176074262,-4.54872398814009,
-43.8446688784225));
#15464=CARTESIAN_POINT('Ctrl Pts',(-9.74928976254991,-4.52937690754481,
-43.8367000449069));
#15465=CARTESIAN_POINT('Ctrl Pts',(-9.75819464297145,-4.51010296781282,
-43.8285626112942));
#15466=CARTESIAN_POINT('Ctrl Pts',(-9.79687625799754,-4.42637953959631,
-43.793214683034));
#15467=CARTESIAN_POINT('Ctrl Pts',(-9.83381278158552,-4.34360625274378,
-43.7545078689066));
#15468=CARTESIAN_POINT('Ctrl Pts',(-9.86916355129727,-4.26172191436226,
-43.7127052463082));
#15469=CARTESIAN_POINT('Ctrl Pts',(-9.88520563768197,-4.22456301681685,
-43.6937353260407));
#15470=CARTESIAN_POINT('Ctrl Pts',(-9.90092094238166,-4.18758710591906,
-43.6741272004195));
#15471=CARTESIAN_POINT('Ctrl Pts',(-9.91632327429604,-4.15078809569386,
-43.6539021212315));
#15472=CARTESIAN_POINT('Ctrl Pts',(-9.92074536029069,-4.14022291708075,
-43.6480954005404));
#15473=CARTESIAN_POINT('Ctrl Pts',(-9.92514262036434,-4.12966998485355,
-43.6422375099564));
#15474=CARTESIAN_POINT('Ctrl Pts',(-9.9295151527142,-4.11912962069311,-43.6363292143049));
#15475=CARTESIAN_POINT('Ctrl Pts',(-9.96375695635676,-4.03658681688429,
-43.590060671645));
#15476=CARTESIAN_POINT('Ctrl Pts',(-9.9965137017754,-3.95469685147143,-43.5405520961091));
#15477=CARTESIAN_POINT('Ctrl Pts',(-10.027746094834,-3.87385088045541,-43.4883126421827));
#15478=CARTESIAN_POINT('Ctrl Pts',(-10.0550083068346,-3.80328184025716,
-43.4427137325806));
#15479=CARTESIAN_POINT('Ctrl Pts',(-10.0811094656341,-3.73350767058796,
-43.3950344466879));
#15480=CARTESIAN_POINT('Ctrl Pts',(-10.1060391066288,-3.66476105295963,
-43.3456209213211));
#15481=CARTESIAN_POINT('Ctrl Pts',(-10.1302917164194,-3.5978814339504,-43.2975493526471));
#15482=CARTESIAN_POINT('Ctrl Pts',(-10.1534368297526,-3.53198496973756,
-43.2478594105366));
#15483=CARTESIAN_POINT('Ctrl Pts',(-10.1755279180874,-3.46715135906702,
-43.1968184788605));
#15484=CARTESIAN_POINT('Ctrl Pts',(-10.2029132662501,-3.38677999057866,
-43.1335452863713));
#15485=CARTESIAN_POINT('Ctrl Pts',(-10.2287275664732,-3.3079046565932,-43.068093899653));
#15486=CARTESIAN_POINT('Ctrl Pts',(-10.2531383411246,-3.23042635910777,
-43.0007320410579));
#15487=CARTESIAN_POINT('Ctrl Pts',(-10.2557783156256,-3.22204724239941,
-42.9934469961721));
#15488=CARTESIAN_POINT('Ctrl Pts',(-10.2584018561637,-3.21368446191673,
-42.9861395599652));
#15489=CARTESIAN_POINT('Ctrl Pts',(-10.2610091614443,-3.20533788995137,
-42.9788100374481));
#15490=CARTESIAN_POINT('Ctrl Pts',(-10.2869627757751,-3.12225451978454,
-42.9058505715778));
#15491=CARTESIAN_POINT('Ctrl Pts',(-10.3113115241216,-3.04077434106176,
-42.8307166031143));
#15492=CARTESIAN_POINT('Ctrl Pts',(-10.3342333296945,-2.96077179059499,
-42.753640700006));
#15493=CARTESIAN_POINT('Ctrl Pts',(-10.3567452030602,-2.88220000098129,
-42.6779432177634));
#15494=CARTESIAN_POINT('Ctrl Pts',(-10.377880537689,-2.80505340505405,-42.6003724327715));
#15495=CARTESIAN_POINT('Ctrl Pts',(-10.397788145182,-2.72920873884206,-42.5210988743318));
#15496=CARTESIAN_POINT('Ctrl Pts',(-10.4182395170266,-2.65129242108953,
-42.4396600062182));
#15497=CARTESIAN_POINT('Ctrl Pts',(-10.4373951504249,-2.57475010585073,
-42.356424239593));
#15498=CARTESIAN_POINT('Ctrl Pts',(-10.4553967161989,-2.4994440912758,-42.2715232304453));
#15499=CARTESIAN_POINT('Ctrl Pts',(-10.4733982819729,-2.42413807670088,
-42.1866222212975));
#15500=CARTESIAN_POINT('Ctrl Pts',(-10.4902456755633,-2.35006832727967,
-42.1000558922966));
#15501=CARTESIAN_POINT('Ctrl Pts',(-10.5060622858798,-2.27709359605911,
-42.0119030752));
#15502=CARTESIAN_POINT('',(-10.5060622858798,2.2770935960591,-42.0119030752));
#15503=CARTESIAN_POINT('Ctrl Pts',(-10.5060622858798,-2.27709359605911,
-42.0119030752));
#15504=CARTESIAN_POINT('Ctrl Pts',(-10.5169211750016,-2.2269928159833,-41.9513817846856));
#15505=CARTESIAN_POINT('Ctrl Pts',(-10.5275918198861,-2.17603932438343,
-41.8916923371475));
#15506=CARTESIAN_POINT('Ctrl Pts',(-10.5380631093571,-2.12409833598685,
-41.8329130265209));
#15507=CARTESIAN_POINT('Ctrl Pts',(-10.5481652864803,-2.07398826442453,
-41.7762056831913));
#15508=CARTESIAN_POINT('Ctrl Pts',(-10.5580819092047,-2.02295908941791,
-41.7203453668008));
#15509=CARTESIAN_POINT('Ctrl Pts',(-10.5677951269423,-1.97088759165573,
-41.6654490466084));
#15510=CARTESIAN_POINT('Ctrl Pts',(-10.5774114727849,-1.91933541352523,
-41.611100218576));
#15511=CARTESIAN_POINT('Ctrl Pts',(-10.5868284809711,-1.86676161176197,
-41.5576959574735));
#15512=CARTESIAN_POINT('Ctrl Pts',(-10.5960207407409,-1.81304431243898,
-41.5053993769468));
#15513=CARTESIAN_POINT('Ctrl Pts',(-10.6089936823863,-1.7372336405342,-41.4315937508633));
#15514=CARTESIAN_POINT('Ctrl Pts',(-10.6215612237893,-1.6588909490796,-41.3597527153406));
#15515=CARTESIAN_POINT('Ctrl Pts',(-10.6335531768026,-1.57807254007726,
-41.2909134876665));
#15516=CARTESIAN_POINT('Ctrl Pts',(-10.6457596887228,-1.49580813562584,
-41.2208425949402));
#15517=CARTESIAN_POINT('Ctrl Pts',(-10.6573697537526,-1.41097862402483,
-41.1538819680966));
#15518=CARTESIAN_POINT('Ctrl Pts',(-10.6682028723582,-1.32364132243195,
-41.0911792922432));
#15519=CARTESIAN_POINT('Ctrl Pts',(-10.6697806490981,-1.31092118449275,
-41.0820470352182));
#15520=CARTESIAN_POINT('Ctrl Pts',(-10.6713419446356,-1.2981478476095,-41.0730051883889));
#15521=CARTESIAN_POINT('Ctrl Pts',(-10.6728862011302,-1.28532148543937,
-41.0640573883661));
#15522=CARTESIAN_POINT('Ctrl Pts',(-10.6781023652254,-1.24199681103724,
-41.0338336571583));
#15523=CARTESIAN_POINT('Ctrl Pts',(-10.6831272007389,-1.19804491020261,
-41.0046644056734));
#15524=CARTESIAN_POINT('Ctrl Pts',(-10.6879474118809,-1.15337770087377,
-40.976644281761));
#15525=CARTESIAN_POINT('Ctrl Pts',(-10.6933301180208,-1.10349804730097,
-40.9453543468218));
#15526=CARTESIAN_POINT('Ctrl Pts',(-10.6984568327903,-1.05272674189745,
-40.9154954419056));
#15527=CARTESIAN_POINT('Ctrl Pts',(-10.703300090004,-1.00093912690731,-40.8872409339168));
#15528=CARTESIAN_POINT('Ctrl Pts',(-10.7080905723239,-0.94971581931515,
-40.8592943031663));
#15529=CARTESIAN_POINT('Ctrl Pts',(-10.7126037747887,-0.897498241347043,
-40.8329170291832));
#15530=CARTESIAN_POINT('Ctrl Pts',(-10.7168049092765,-0.844163412723419,
-40.808327684429));
#15531=CARTESIAN_POINT('Ctrl Pts',(-10.7210060437642,-0.790828584099796,
-40.7837383396748));
#15532=CARTESIAN_POINT('Ctrl Pts',(-10.7248951650162,-0.73637652235252,
-40.7609365199596));
#15533=CARTESIAN_POINT('Ctrl Pts',(-10.7284285456406,-0.680681659397462,
-40.7401970252461));
#15534=CARTESIAN_POINT('Ctrl Pts',(-10.7305548947967,-0.647165110394726,
-40.7277162280239));
#15535=CARTESIAN_POINT('Ctrl Pts',(-10.7325374851499,-0.613428835245424,
-40.7160697181704));
#15536=CARTESIAN_POINT('Ctrl Pts',(-10.7343701088873,-0.579481117404477,
-40.7052989261484));
#15537=CARTESIAN_POINT('Ctrl Pts',(-10.7387885965857,-0.497632579372944,
-40.6793303592902));
#15538=CARTESIAN_POINT('Ctrl Pts',(-10.7423340227891,-0.414554739665019,
-40.6584535425089));
#15539=CARTESIAN_POINT('Ctrl Pts',(-10.7449224741416,-0.330365449223965,
-40.6432014555172));
#15540=CARTESIAN_POINT('Ctrl Pts',(-10.7453420295562,-0.316719423917338,
-40.6407292840096));
#15541=CARTESIAN_POINT('Ctrl Pts',(-10.745736463536,-0.303044203764577,
-40.6384047780912));
#15542=CARTESIAN_POINT('Ctrl Pts',(-10.7461054430156,-0.289340297214281,
-40.6362300776288));
#15543=CARTESIAN_POINT('Ctrl Pts',(-10.7480705739512,-0.216355288052297,
-40.6246479398935));
#15544=CARTESIAN_POINT('Ctrl Pts',(-10.7493119495664,-0.14241824380966,
-40.6173253496218));
#15545=CARTESIAN_POINT('Ctrl Pts',(-10.7497839186023,-0.0680262630204308,
-40.614541089547));
#15546=CARTESIAN_POINT('Ctrl Pts',(-10.7499255932274,-0.0456954421490946,
-40.6137053164929));
#15547=CARTESIAN_POINT('Ctrl Pts',(-10.7499979808866,-0.0233238925964778,
-40.6132782374545));
#15548=CARTESIAN_POINT('Ctrl Pts',(-10.749999956258,-0.000925701714180853,
-40.6132667624236));
#15549=CARTESIAN_POINT('Ctrl Pts',(-10.750000064608,0.000302849218660908,
-40.613266133013));
#15550=CARTESIAN_POINT('Ctrl Pts',(-10.7499999611065,0.00153120719642892,
-40.6132667505364));
#15551=CARTESIAN_POINT('Ctrl Pts',(-10.7499996458546,0.00275937048380377,
-40.6132686144898));
#15552=CARTESIAN_POINT('Ctrl Pts',(-10.7499763020177,0.0937026634470254,
-40.6134066369061));
#15553=CARTESIAN_POINT('Ctrl Pts',(-10.7488040773026,0.183579345376722,
-40.6203491177147));
#15554=CARTESIAN_POINT('Ctrl Pts',(-10.7465539700609,0.272461900589267,
-40.6336315852736));
#15555=CARTESIAN_POINT('Ctrl Pts',(-10.7459490926706,0.296355449772789,
-40.6372021992274));
#15556=CARTESIAN_POINT('Ctrl Pts',(-10.7452662792949,0.320177132210481,
-40.6412312609462));
#15557=CARTESIAN_POINT('Ctrl Pts',(-10.7445068169311,0.343928299168354,
-40.6457103741471));
#15558=CARTESIAN_POINT('Ctrl Pts',(-10.7431254287457,0.387129362169936,
-40.6538574454859));
#15559=CARTESIAN_POINT('Ctrl Pts',(-10.741485265122,0.430235670199365,-40.6635240587775));
#15560=CARTESIAN_POINT('Ctrl Pts',(-10.7395996435294,0.473061091575405,
-40.674624855102));
#15561=CARTESIAN_POINT('Ctrl Pts',(-10.7376799648323,0.516660003163934,
-40.685926148165));
#15562=CARTESIAN_POINT('Ctrl Pts',(-10.7355058809133,0.559967790910228,
-40.6987138561558));
#15563=CARTESIAN_POINT('Ctrl Pts',(-10.7331007175571,0.602790413091531,
-40.7128442814695));
#15564=CARTESIAN_POINT('Ctrl Pts',(-10.7316726009835,0.628217250027148,
-40.7212345201327));
#15565=CARTESIAN_POINT('Ctrl Pts',(-10.7301631907923,0.653473079836672,
-40.730097134421));
#15566=CARTESIAN_POINT('Ctrl Pts',(-10.7285788584156,0.67851765769429,-40.7393935351316));
#15567=CARTESIAN_POINT('Ctrl Pts',(-10.7249879199081,0.735281970761078,
-40.7604641158909));
#15568=CARTESIAN_POINT('Ctrl Pts',(-10.7210180162077,0.790886302064723,
-40.783725776146));
#15569=CARTESIAN_POINT('Ctrl Pts',(-10.7167121853542,0.845441367712903,
-40.8089128341746));
#15570=CARTESIAN_POINT('Ctrl Pts',(-10.712274675129,0.901664816770976,-40.8348701537593));
#15571=CARTESIAN_POINT('Ctrl Pts',(-10.7074803696864,0.956773839390786,
-40.8628725267494));
#15572=CARTESIAN_POINT('Ctrl Pts',(-10.7023673177639,1.01088733787075,-40.8926847844663));
#15573=CARTESIAN_POINT('Ctrl Pts',(-10.69775747029,1.05967521995343,-40.9195630487621));
#15574=CARTESIAN_POINT('Ctrl Pts',(-10.6928883872567,1.10765384988097,-40.9479133723767));
#15575=CARTESIAN_POINT('Ctrl Pts',(-10.6877820642804,1.15490889098301,-40.977599136389));
#15576=CARTESIAN_POINT('Ctrl Pts',(-10.6830090262702,1.19907963936724,-41.0053473381089));
#15577=CARTESIAN_POINT('Ctrl Pts',(-10.6780286317076,1.24261786862674,-41.0342600437575));
#15578=CARTESIAN_POINT('Ctrl Pts',(-10.6728534474259,1.28559264108763,-41.0642459908329));
#15579=CARTESIAN_POINT('Ctrl Pts',(-10.6660559159946,1.34203939750374,-41.1036321086305));
#15580=CARTESIAN_POINT('Ctrl Pts',(-10.658962501078,1.39718157663253,-41.1446412939523));
#15581=CARTESIAN_POINT('Ctrl Pts',(-10.6516162897416,1.45111909578012,-41.1869955273223));
#15582=CARTESIAN_POINT('Ctrl Pts',(-10.6441188346133,1.50616708051922,-41.2302217496076));
#15583=CARTESIAN_POINT('Ctrl Pts',(-10.6363580511712,1.55996028343958,-41.2748491853959));
#15584=CARTESIAN_POINT('Ctrl Pts',(-10.6283717818543,1.61260256544954,-41.3206366361582));
#15585=CARTESIAN_POINT('Ctrl Pts',(-10.6201468071409,1.66681829762756,-41.3677926497818));
#15586=CARTESIAN_POINT('Ctrl Pts',(-10.6116826613633,1.71981327495423,-41.4161791961904));
#15587=CARTESIAN_POINT('Ctrl Pts',(-10.603012462611,1.77169857534448,-41.465587270585));
#15588=CARTESIAN_POINT('Ctrl Pts',(-10.6006686230707,1.78572487648107,-41.4789438961576));
#15589=CARTESIAN_POINT('Ctrl Pts',(-10.5983096802437,1.79967006975955,-41.4923754677647));
#15590=CARTESIAN_POINT('Ctrl Pts',(-10.5959361902354,1.813536321744,-41.5058784916076));
#15591=CARTESIAN_POINT('Ctrl Pts',(-10.5866134040062,1.86800130899971,-41.5589167619592));
#15592=CARTESIAN_POINT('Ctrl Pts',(-10.5770540804843,1.92132307652416,-41.6131249930469));
#15593=CARTESIAN_POINT('Ctrl Pts',(-10.5672843422973,1.97362269097949,-41.6683345047717));
#15594=CARTESIAN_POINT('Ctrl Pts',(-10.5571735077314,2.02774827136858,-41.7254715773146));
#15595=CARTESIAN_POINT('Ctrl Pts',(-10.5468373130892,2.08077907582018,-41.7836811722096));
#15596=CARTESIAN_POINT('Ctrl Pts',(-10.5362955537602,2.13284690400159,-41.8428326535671));
#15597=CARTESIAN_POINT('Ctrl Pts',(-10.5263960333759,2.18174258738393,-41.898380430478));
#15598=CARTESIAN_POINT('Ctrl Pts',(-10.5163151222045,2.22978902446844,-41.9547595793156));
#15599=CARTESIAN_POINT('Ctrl Pts',(-10.5060622858798,2.27709359605911,-42.0119030752));
#15600=CARTESIAN_POINT('Ctrl Pts',(-10.5060622858798,2.27709359605911,-42.0119030752));
#15601=CARTESIAN_POINT('Ctrl Pts',(-10.4903858538268,2.34942157232421,-42.0992746181415));
#15602=CARTESIAN_POINT('Ctrl Pts',(-10.4736968030168,2.42282523877712,-42.1850875945395));
#15603=CARTESIAN_POINT('Ctrl Pts',(-10.4558750724622,2.49744213415037,-42.2692654755765));
#15604=CARTESIAN_POINT('Ctrl Pts',(-10.4383088490782,2.57098925957247,-42.3522365124096));
#15605=CARTESIAN_POINT('Ctrl Pts',(-10.4196422455203,2.64571509992633,-42.4336189548605));
#15606=CARTESIAN_POINT('Ctrl Pts',(-10.3997435370008,2.72174811674475,-42.5132910675444));
#15607=CARTESIAN_POINT('Ctrl Pts',(-10.3794106774459,2.79944002579496,-42.594701470439));
#15608=CARTESIAN_POINT('Ctrl Pts',(-10.3577915446787,2.8784968272504,-42.6743263559687));
#15609=CARTESIAN_POINT('Ctrl Pts',(-10.3347260481214,2.95905154530767,-42.7519828654194));
#15610=CARTESIAN_POINT('Ctrl Pts',(-10.3116605515641,3.03960626336494,-42.8296393748701));
#15611=CARTESIAN_POINT('Ctrl Pts',(-10.2871488217201,3.12165894477404,-42.90532756893));
#15612=CARTESIAN_POINT('Ctrl Pts',(-10.2610091614501,3.20533788993294,-42.9788100375568));
#15613=CARTESIAN_POINT('Ctrl Pts',(-10.2369004525634,3.28251530187875,-43.0465832001037));
#15614=CARTESIAN_POINT('Ctrl Pts',(-10.211405190032,3.36107882836898,-43.1124719480175));
#15615=CARTESIAN_POINT('Ctrl Pts',(-10.1843579213645,3.44112785947417,-43.1762137875333));
#15616=CARTESIAN_POINT('Ctrl Pts',(-10.181433339459,3.4497834450271,-43.1831061001274));
#15617=CARTESIAN_POINT('Ctrl Pts',(-10.1784905933341,3.45845639526925,-43.1899732648956));
#15618=CARTESIAN_POINT('Ctrl Pts',(-10.1755294601892,3.46714683325539,-43.1968149158649));
#15619=CARTESIAN_POINT('Ctrl Pts',(-10.1534379069393,3.53198190285271,-43.2478570977966));
#15620=CARTESIAN_POINT('Ctrl Pts',(-10.1302922806711,3.5978798779554,-43.2975482341483));
#15621=CARTESIAN_POINT('Ctrl Pts',(-10.1060391066289,3.6647610529594,-43.3456209213228));
#15622=CARTESIAN_POINT('Ctrl Pts',(-10.0774789910328,3.74351916049569,-43.4022304809757));
#15623=CARTESIAN_POINT('Ctrl Pts',(-10.0473808013863,3.82362678346992,-43.4565636983887));
#15624=CARTESIAN_POINT('Ctrl Pts',(-10.0157618677232,3.90473120961818,-43.5081008021272));
#15625=CARTESIAN_POINT('Ctrl Pts',(-9.98816221632845,3.97552594014595,-43.5530866992554));
#15626=CARTESIAN_POINT('Ctrl Pts',(-9.95940424479242,4.04707940133543,-43.5959421869829));
#15627=CARTESIAN_POINT('Ctrl Pts',(-9.9295151528399,4.1191296203901,-43.6363292172957));
#15628=CARTESIAN_POINT('Ctrl Pts',(-9.92514363536074,4.12966753811858,-43.6422361417758));
#15629=CARTESIAN_POINT('Ctrl Pts',(-9.92074740166516,4.14021801800824,-43.6480926845505));
#15630=CARTESIAN_POINT('Ctrl Pts',(-9.91632635362655,4.15078073859803,-43.653898081326));
#15631=CARTESIAN_POINT('Ctrl Pts',(-9.88238540720856,4.23187208400656,-43.6984668485442));
#15632=CARTESIAN_POINT('Ctrl Pts',(-9.84692571292298,4.31382280716079,-43.7400429324949));
#15633=CARTESIAN_POINT('Ctrl Pts',(-9.80979522522875,4.39669658013697,-43.7783856209135));
#15634=CARTESIAN_POINT('Ctrl Pts',(-9.79294577201636,4.4343038901135,-43.795785158993));
#15635=CARTESIAN_POINT('Ctrl Pts',(-9.7757520459721,4.47210120715835,-43.8125181941863));
#15636=CARTESIAN_POINT('Ctrl Pts',(-9.75819873711372,4.5100941063408,-43.8285588699776));
#15637=CARTESIAN_POINT('Ctrl Pts',(-9.73442906213716,4.56154189161422,-43.8502802247968));
#15638=CARTESIAN_POINT('Ctrl Pts',(-9.70992373940938,4.61351031126775,-43.8707967158355));
#15639=CARTESIAN_POINT('Ctrl Pts',(-9.6847544078432,4.66577026911174,-43.8899311961925));
#15640=CARTESIAN_POINT('Ctrl Pts',(-9.65977375931941,4.7176384577975,-43.9089222340446));
#15641=CARTESIAN_POINT('Ctrl Pts',(-9.63413899470648,4.76979381628853,-43.926551869351));
#15642=CARTESIAN_POINT('Ctrl Pts',(-9.60793275938919,4.82201931451656,-43.9426963378991));
#15643=CARTESIAN_POINT('Ctrl Pts',(-9.59807555103569,4.84166340345821,-43.9487689152193));
#15644=CARTESIAN_POINT('Ctrl Pts',(-9.58813762048344,4.86131748759562,-43.9546318746603));
#15645=CARTESIAN_POINT('Ctrl Pts',(-9.57812384114842,4.88097027922769,-43.9602804639433));
#15646=CARTESIAN_POINT('Ctrl Pts',(-9.47988016966834,5.07378083957379,-44.0156979173622));
#15647=CARTESIAN_POINT('Ctrl Pts',(-9.37498500801622,5.2652020058733,-44.0501809839947));
#15648=CARTESIAN_POINT('Ctrl Pts',(-9.26310468387546,5.45512072549868,-44.0630753330053));
#15649=CARTESIAN_POINT('Ctrl Pts',(-9.23044829916616,5.51055548419478,-44.0668390226898));
#15650=CARTESIAN_POINT('Ctrl Pts',(-9.1971967973383,5.56586196087343,-44.068763589347));
#15651=CARTESIAN_POINT('Ctrl Pts',(-9.16334192291166,5.62103668404923,-44.0688332970512));
#15652=CARTESIAN_POINT('Ctrl Pts',(-9.13431980327369,5.66833526199759,-44.0688930540393));
#15653=CARTESIAN_POINT('Ctrl Pts',(-9.10476428938528,5.71568116575354,-44.0675714534323));
#15654=CARTESIAN_POINT('Ctrl Pts',(-9.07480312871392,5.76285537335515,-44.0648683451568));
#15655=CARTESIAN_POINT('Ctrl Pts',(-9.05948004307237,5.78698175587688,-44.0634858900491));
#15656=CARTESIAN_POINT('Ctrl Pts',(-9.0440510769082,5.81106335134616,-44.0617428892334));
#15657=CARTESIAN_POINT('Ctrl Pts',(-9.02853471299321,5.83507163077762,-44.0596443418482));
#15658=CARTESIAN_POINT('Ctrl Pts',(-8.99820642947174,5.88199821160859,-44.0555425213169));
#15659=CARTESIAN_POINT('Ctrl Pts',(-8.96754046580899,5.92864274808946,-44.0500576047011));
#15660=CARTESIAN_POINT('Ctrl Pts',(-8.93668327281746,5.97479695215066,-44.0432501377108));
#15661=CARTESIAN_POINT('Ctrl Pts',(-8.93450940683793,5.9780484810259,-44.0427705567942));
#15662=CARTESIAN_POINT('Ctrl Pts',(-8.93233459747615,5.98129757948464,-44.0422844323533));
#15663=CARTESIAN_POINT('Ctrl Pts',(-8.93015889852948,5.98454417612995,-44.0417917948209));
#15664=CARTESIAN_POINT('Ctrl Pts',(-8.87228268877595,6.07090755315709,-44.0286870437247));
#15665=CARTESIAN_POINT('Ctrl Pts',(-8.81378786331539,6.15548448285379,-44.0109788675573));
#15666=CARTESIAN_POINT('Ctrl Pts',(-8.75476238687981,6.23831993001948,-43.9890041642549));
#15667=CARTESIAN_POINT('Ctrl Pts',(-8.73245078970821,6.26963168284721,-43.9806977386628));
#15668=CARTESIAN_POINT('Ctrl Pts',(-8.71004631052317,6.30071602093432,-43.9717711696744));
#15669=CARTESIAN_POINT('Ctrl Pts',(-8.68756771503179,6.33155719715214,-43.9622493672937));
#15670=CARTESIAN_POINT('Ctrl Pts',(-8.63693389294267,6.40102802464363,-43.9408011745944));
#15671=CARTESIAN_POINT('Ctrl Pts',(-8.58568689339014,6.46958806021716,-43.9162245598074));
#15672=CARTESIAN_POINT('Ctrl Pts',(-8.53411477764999,6.53692068556944,-43.8887772589389));
#15673=CARTESIAN_POINT('Ctrl Pts',(-8.50992046466342,6.56850881393301,-43.8759007542945));
#15674=CARTESIAN_POINT('Ctrl Pts',(-8.48565461088127,6.59982718080281,-43.8623930899239));
#15675=CARTESIAN_POINT('Ctrl Pts',(-8.46134684828156,6.63084530909281,-43.8482841546581));
#15676=CARTESIAN_POINT('Ctrl Pts',(-8.40630859605882,6.70107734140343,-43.8163383458011));
#15677=CARTESIAN_POINT('Ctrl Pts',(-8.35113317820789,6.76968547688455,-43.7813828522151));
#15678=CARTESIAN_POINT('Ctrl Pts',(-8.29600947450433,6.83657937895735,-43.7437667181145));
#15679=CARTESIAN_POINT('Ctrl Pts',(-8.25940112996534,6.8810044601857,-43.7187853706205));
#15680=CARTESIAN_POINT('Ctrl Pts',(-8.2228158170931,6.92467378380488,-43.6926316589512));
#15681=CARTESIAN_POINT('Ctrl Pts',(-8.18631127030155,6.96756410281872,-43.6654197758277));
#15682=CARTESIAN_POINT('Ctrl Pts',(-8.12642898534358,7.03792164813465,-43.6207812339838));
#15683=CARTESIAN_POINT('Ctrl Pts',(-8.06676026536866,7.10619090896555,-43.5733019776527));
#15684=CARTESIAN_POINT('Ctrl Pts',(-8.00730071472196,7.17256758947688,-43.5232728467746));
#15685=CARTESIAN_POINT('Ctrl Pts',(-7.94784116407525,7.23894426998821,-43.4732437158965));
#15686=CARTESIAN_POINT('Ctrl Pts',(-7.88859071458996,7.30342827304339,-43.4206643974427));
#15687=CARTESIAN_POINT('Ctrl Pts',(-7.82953376242379,7.36619990657248,-43.3657719705771));
#15688=CARTESIAN_POINT('Ctrl Pts',(-7.78246051217648,7.4162340635204,-43.322018189663));
#15689=CARTESIAN_POINT('Ctrl Pts',(-7.73551173823807,7.46518289020163,-43.2768135657473));
#15690=CARTESIAN_POINT('Ctrl Pts',(-7.68867196096474,7.51312673470195,-43.2302274255208));
#15691=CARTESIAN_POINT('Ctrl Pts',(-7.62941400081416,7.57378147288071,-43.1712903467852));
#15692=CARTESIAN_POINT('Ctrl Pts',(-7.57024340360777,7.63291386978282,-43.1100539400581));
#15693=CARTESIAN_POINT('Ctrl Pts',(-7.51134952911368,7.69045086718029,-43.0468902512885));
#15694=CARTESIAN_POINT('Ctrl Pts',(-7.4510109777538,7.74939925701512,-42.982177146375));
#15695=CARTESIAN_POINT('Ctrl Pts',(-7.39096291979704,7.80667305854691,-42.9154410888264));
#15696=CARTESIAN_POINT('Ctrl Pts',(-7.33141801291965,7.86220712589153,-42.8471352400235));
#15697=CARTESIAN_POINT('Ctrl Pts',(-7.28787285723929,7.90281915696019,-42.7971832126213));
#15698=CARTESIAN_POINT('Ctrl Pts',(-7.24459698068532,7.94250106993998,-42.7463928033134));
#15699=CARTESIAN_POINT('Ctrl Pts',(-7.20167632415047,7.98123150622077,-42.6949580898005));
#15700=CARTESIAN_POINT('Ctrl Pts',(-7.13930068922744,8.03751758730387,-42.6202091653556));
#15701=CARTESIAN_POINT('Ctrl Pts',(-7.07752996216333,8.0919282723007,-42.5439257142954));
#15702=CARTESIAN_POINT('Ctrl Pts',(-7.01632524907499,8.14464761374309,-42.4662769768287));
#15703=CARTESIAN_POINT('Ctrl Pts',(-6.95400229907961,8.19833016063715,-42.3872095629296));
#15704=CARTESIAN_POINT('Ctrl Pts',(-6.89226620628615,8.25025895340072,-42.3067264625329));
#15705=CARTESIAN_POINT('Ctrl Pts',(-6.83106473213676,8.30061305897572,-42.2249555224749));
#15706=CARTESIAN_POINT('Ctrl Pts',(-6.7992606944567,8.32678013898989,-42.1824623293798));
#15707=CARTESIAN_POINT('Ctrl Pts',(-6.76760085008768,8.35252173360003,-42.1396205349761));
#15708=CARTESIAN_POINT('Ctrl Pts',(-6.73607674834659,8.37786144795107,-42.0964428903666));
#15709=CARTESIAN_POINT('Ctrl Pts',(-6.67199336517252,8.42937297515064,-42.0086697456537));
#15710=CARTESIAN_POINT('Ctrl Pts',(-6.60851060515526,8.4791932576852,-41.9195563684028));
#15711=CARTESIAN_POINT('Ctrl Pts',(-6.5455713594808,8.52749545018427,-41.8292245834422));
#15712=CARTESIAN_POINT('Ctrl Pts',(-6.49978585110939,8.56263315187302,-41.7635122182526));
#15713=CARTESIAN_POINT('Ctrl Pts',(-6.45428772303884,8.59696718415172,-41.6971540009845));
#15714=CARTESIAN_POINT('Ctrl Pts',(-6.40905142763636,8.63055964574466,-41.6301805545832));
#15715=CARTESIAN_POINT('Ctrl Pts',(-6.35304742562662,8.67214820355701,-41.547265254082));
#15716=CARTESIAN_POINT('Ctrl Pts',(-6.29738512256274,8.71263450157332,-41.4632867948496));
#15717=CARTESIAN_POINT('Ctrl Pts',(-6.24209165713335,8.7520699926184,-41.3783888757593));
#15718=CARTESIAN_POINT('Ctrl Pts',(-6.18469410966926,8.7930061222578,-41.290260336469));
#15719=CARTESIAN_POINT('Ctrl Pts',(-6.12769384861597,8.83281008906891,-41.2011409061342));
#15720=CARTESIAN_POINT('Ctrl Pts',(-6.07110079547896,8.87154004988281,-41.1111391345468));
#15721=CARTESIAN_POINT('Ctrl Pts',(-6.05484968628221,8.88266164144722,-41.0852944674562));
#15722=CARTESIAN_POINT('Ctrl Pts',(-6.03863203884112,8.89369466753796,-41.0593767314042));
#15723=CARTESIAN_POINT('Ctrl Pts',(-6.02244782123308,8.90464048912287,-41.0333877658703));
#15724=CARTESIAN_POINT('Ctrl Pts',(-5.96789208360469,8.94153800156218,-40.9457809862758));
#15725=CARTESIAN_POINT('Ctrl Pts',(-5.91381192380442,8.97738468492173,-40.857526983766));
#15726=CARTESIAN_POINT('Ctrl Pts',(-5.86012825014004,9.01229190082103,-40.7685826949025));
#15727=CARTESIAN_POINT('Ctrl Pts',(-5.78173848263234,9.06326398137933,-40.6387048074699));
#15728=CARTESIAN_POINT('Ctrl Pts',(-5.70446841167726,9.1120548788626,-40.5078066310337));
#15729=CARTESIAN_POINT('Ctrl Pts',(-5.62824515844005,9.15889493533549,-40.3760464765598));
#15730=CARTESIAN_POINT('Ctrl Pts',(-5.5506816632265,9.2065585857537,-40.2419695685711));
#15731=CARTESIAN_POINT('Ctrl Pts',(-5.47420216130162,9.25220373229958,-40.1070075565167));
#15732=CARTESIAN_POINT('Ctrl Pts',(-5.39872201472086,9.29604069694951,-39.9712454668733));
#15733=CARTESIAN_POINT('Ctrl Pts',(-5.32192875420435,9.34064028504136,-39.833121549651));
#15734=CARTESIAN_POINT('Ctrl Pts',(-5.24616988273066,9.38336814459259,-39.6941694463143));
#15735=CARTESIAN_POINT('Ctrl Pts',(-5.1713497664352,9.4244226701412,-39.5544301784892));
#15736=CARTESIAN_POINT('Ctrl Pts',(-5.13294490279669,9.44549579236426,-39.4827025764554));
#15737=CARTESIAN_POINT('Ctrl Pts',(-5.09478727512359,9.46612767452138,-39.4107668025937));
#15738=CARTESIAN_POINT('Ctrl Pts',(-5.05686335325565,9.486342957516,-39.3386236125289));
#15739=CARTESIAN_POINT('Ctrl Pts',(-4.97902793754477,9.52783299541552,-39.1905562473193));
#15740=CARTESIAN_POINT('Ctrl Pts',(-4.90219178004792,9.56756126829927,-39.0416213059115));
#15741=CARTESIAN_POINT('Ctrl Pts',(-4.82630358622753,9.60569069322788,-38.8919330766784));
#15742=CARTESIAN_POINT('Ctrl Pts',(-4.73610193391763,9.65101180257367,-38.7140117831485));
#15743=CARTESIAN_POINT('Ctrl Pts',(-4.64723779752275,9.69407935976452,-38.5350724274354));
#15744=CARTESIAN_POINT('Ctrl Pts',(-4.55961797925815,9.7351250216472,-38.355165386151));
#15745=CARTESIAN_POINT('Ctrl Pts',(-4.47869953946941,9.77303141069736,-38.1890180763747));
#15746=CARTESIAN_POINT('Ctrl Pts',(-4.39884221195997,9.8092129796294,-38.0220450108315));
#15747=CARTESIAN_POINT('Ctrl Pts',(-4.3199665599412,9.84383312150183,-37.8542518249589));
#15748=CARTESIAN_POINT('Ctrl Pts',(-4.2188499945973,9.888215256524,-37.6391452589997));
#15749=CARTESIAN_POINT('Ctrl Pts',(-4.11934342920786,9.93003289724634,-37.4227359175084));
#15750=CARTESIAN_POINT('Ctrl Pts',(-4.02137300417359,9.96955084295721,-37.2051666039132));
#15751=CARTESIAN_POINT('Ctrl Pts',(-3.92418102109437,10.0087547915929,-36.9893260271463));
#15752=CARTESIAN_POINT('Ctrl Pts',(-3.82850078232874,10.0456952252387,-36.7723438791378));
#15753=CARTESIAN_POINT('Ctrl Pts',(-3.73425145270028,10.0806028780621,-36.5543157476452));
#15754=CARTESIAN_POINT('Ctrl Pts',(-3.6388698131308,10.1159299108691,-36.3336682296626));
#15755=CARTESIAN_POINT('Ctrl Pts',(-3.54495362434385,10.1491749111289,-36.1119496056389));
#15756=CARTESIAN_POINT('Ctrl Pts',(-3.45241105969329,10.1805508308907,-35.8892121412572));
#15757=CARTESIAN_POINT('Ctrl Pts',(-3.35986849504272,10.2119267506525,-35.6664746768756));
#15758=CARTESIAN_POINT('Ctrl Pts',(-3.26869949926948,10.2414334401001,-35.4427184156392));
#15759=CARTESIAN_POINT('Ctrl Pts',(-3.17880504329257,10.269259880679,-35.217947694751));
#15760=CARTESIAN_POINT('Ctrl Pts',(-3.11875845584136,10.2878470424735,-35.0678081271702));
#15761=CARTESIAN_POINT('Ctrl Pts',(-3.05925105749581,10.3056863347945,-34.9170987408756));
#15762=CARTESIAN_POINT('Ctrl Pts',(-3.00037766351568,10.3227975174792,-34.7661332394234));
#15763=CARTESIAN_POINT('Ctrl Pts',(-2.93300394142254,10.3423792672126,-34.5933708581017));
#15764=CARTESIAN_POINT('Ctrl Pts',(-2.86626401986577,10.3610642855877,-34.4197841784193));
#15765=CARTESIAN_POINT('Ctrl Pts',(-2.80032934319939,10.378855683455,-34.2458784964172));
#15766=CARTESIAN_POINT('Ctrl Pts',(-2.78727949791908,10.382376971512,-34.2114589412114));
#15767=CARTESIAN_POINT('Ctrl Pts',(-2.77426113533288,10.3858632617364,-34.1770267380782));
#15768=CARTESIAN_POINT('Ctrl Pts',(-2.76127549568886,10.3893145893709,-34.1425855826182));
#15769=CARTESIAN_POINT('Ctrl Pts',(-2.6314416794453,10.4238218643432,-33.7982339163321));
#15770=CARTESIAN_POINT('Ctrl Pts',(-2.50457200276917,10.4549409997331,-33.4522457849824));
#15771=CARTESIAN_POINT('Ctrl Pts',(-2.38057046165633,10.4830999538713,-33.1049548971784));
#15772=CARTESIAN_POINT('Ctrl Pts',(-2.36970090271685,10.4855682732884,-33.0745125434766));
#15773=CARTESIAN_POINT('Ctrl Pts',(-2.35885337846789,10.4880138159116,-33.0440601712045));
#15774=CARTESIAN_POINT('Ctrl Pts',(-2.34802782249455,10.4904368519567,-33.0135979999787));
#15775=CARTESIAN_POINT('Ctrl Pts',(-2.21770246908197,10.519606996168,-32.6468738113555));
#15776=CARTESIAN_POINT('Ctrl Pts',(-2.09055855127056,10.5455214163779,-32.2787518270953));
#15777=CARTESIAN_POINT('Ctrl Pts',(-1.96649166385433,10.5686065331645,-31.9094939632878));
#15778=CARTESIAN_POINT('Ctrl Pts',(-1.92802618510459,10.5757638020191,-31.7950099070721));
#15779=CARTESIAN_POINT('Ctrl Pts',(-1.88985642820042,10.582648729828,-31.6804166865482));
#15780=CARTESIAN_POINT('Ctrl Pts',(-1.85197914734771,10.5892730327154,-31.5657221242989));
#15781=CARTESIAN_POINT('Ctrl Pts',(-1.74502317759923,10.6079784076337,-31.2418533603832));
#15782=CARTESIAN_POINT('Ctrl Pts',(-1.64035044949552,10.6246161413583,-30.9170110061711));
#15783=CARTESIAN_POINT('Ctrl Pts',(-1.53788875472713,10.6394265906663,-30.5913659316414));
#15784=CARTESIAN_POINT('Ctrl Pts',(-1.41260154981738,10.6575363808806,-30.1931765275653));
#15785=CARTESIAN_POINT('Ctrl Pts',(-1.29061928900833,10.6729130832165,-29.7937918410448));
#15786=CARTESIAN_POINT('Ctrl Pts',(-1.17182931752389,10.685939629466,-29.3933438451799));
#15787=CARTESIAN_POINT('Ctrl Pts',(-1.06436790248444,10.697723882594,-29.0310850808448));
#15788=CARTESIAN_POINT('Ctrl Pts',(-0.95951868263359,10.7075839906085,-28.6679570012007));
#15789=CARTESIAN_POINT('Ctrl Pts',(-0.857192809199198,10.7157695937709,
-28.3040700635745));
#15790=CARTESIAN_POINT('Ctrl Pts',(-0.822247336604825,10.7185650721908,
-28.1797984538686));
#15791=CARTESIAN_POINT('Ctrl Pts',(-0.787596463964514,10.7211649655967,
-28.0554372461487));
#15792=CARTESIAN_POINT('Ctrl Pts',(-0.753236825127355,10.7235784272452,
-27.9309927285396));
#15793=CARTESIAN_POINT('Ctrl Pts',(-0.636205486739687,10.7317988467963,
-27.5071259783731));
#15794=CARTESIAN_POINT('Ctrl Pts',(-0.522567636184466,10.7378574576102,
-27.0822064813511));
#15795=CARTESIAN_POINT('Ctrl Pts',(-0.412205680124944,10.7420921052949,
-26.6564401459256));
#15796=CARTESIAN_POINT('Ctrl Pts',(-0.334985886452765,10.7450550703614,
-26.3585332426048));
#15797=CARTESIAN_POINT('Ctrl Pts',(-0.259459080010432,10.7471216957,-26.0605548690474));
#15798=CARTESIAN_POINT('Ctrl Pts',(-0.185425503965189,10.7483995045071,
-25.7619706855148));
#15799=CARTESIAN_POINT('Ctrl Pts',(-0.122586233044267,10.749484101228,-25.5085341584148));
#15800=CARTESIAN_POINT('Ctrl Pts',(-0.0608224949761656,10.75,-25.2546607352261));
#15801=CARTESIAN_POINT('Ctrl Pts',(1.14715432465305E-15,10.75,-25.));
#15802=CARTESIAN_POINT('',(10.5060622858798,2.27709359605911,-42.0119030752));
#15803=CARTESIAN_POINT('Ctrl Pts',(1.18948320324198E-15,10.75,-25.));
#15804=CARTESIAN_POINT('Ctrl Pts',(0.107236928162667,10.75,-25.4489956383632));
#15805=CARTESIAN_POINT('Ctrl Pts',(0.217860527654828,10.7483974074937,-25.8972288302672));
#15806=CARTESIAN_POINT('Ctrl Pts',(0.332035265413112,10.7448689509315,-26.3445236198006));
#15807=CARTESIAN_POINT('Ctrl Pts',(0.441369846116192,10.7414900746027,-26.772856447399));
#15808=CARTESIAN_POINT('Ctrl Pts',(0.55396105844135,10.7363452341562,-27.2003277454457));
#15809=CARTESIAN_POINT('Ctrl Pts',(0.669944681770897,10.729103761743,-27.6267852378145));
#15810=CARTESIAN_POINT('Ctrl Pts',(0.69753293567855,10.7273812808111,-27.7282238482195));
#15811=CARTESIAN_POINT('Ctrl Pts',(0.725313081382595,10.7255399552622,-27.8296051467404));
#15812=CARTESIAN_POINT('Ctrl Pts',(0.753286850732499,10.7235749134872,-27.9309272015895));
#15813=CARTESIAN_POINT('Ctrl Pts',(0.867733545684342,10.7155355057914,-28.3454574766542));
#15814=CARTESIAN_POINT('Ctrl Pts',(0.985408417913843,10.7054316754648,-28.7590760984061));
#15815=CARTESIAN_POINT('Ctrl Pts',(1.10644537549551,10.692907376999,-29.1716055675506));
#15816=CARTESIAN_POINT('Ctrl Pts',(1.22118601156182,10.6810345903645,-29.562675325346));
#15817=CARTESIAN_POINT('Ctrl Pts',(1.33894815037538,10.6669865555207,-29.9527656106568));
#15818=CARTESIAN_POINT('Ctrl Pts',(1.45983743180848,10.6504165882816,-30.3417420854264));
#15819=CARTESIAN_POINT('Ctrl Pts',(1.48571264641705,10.6468699425138,-30.4249988443635));
#15820=CARTESIAN_POINT('Ctrl Pts',(1.51173109034313,10.6432075943476,-30.5082046616496));
#15821=CARTESIAN_POINT('Ctrl Pts',(1.53789373804599,10.6394258703538,-30.5913583746403));
#15822=CARTESIAN_POINT('Ctrl Pts',(1.64034562245794,10.6246167900997,-30.916984996552));
#15823=CARTESIAN_POINT('Ctrl Pts',(1.74501002043019,10.6079804855204,-31.2418078298122));
#15824=CARTESIAN_POINT('Ctrl Pts',(1.85195771749001,10.5892767805306,-31.5656535771417));
#15825=CARTESIAN_POINT('Ctrl Pts',(1.97412810454714,10.5679108330552,-31.9355947856553));
#15826=CARTESIAN_POINT('Ctrl Pts',(2.09934183075205,10.543837289415,-32.3044816614734));
#15827=CARTESIAN_POINT('Ctrl Pts',(2.22770551319777,10.5166457094501,-32.6720516065798));
#15828=CARTESIAN_POINT('Ctrl Pts',(2.26750916253881,10.5082140090398,-32.7860295240449));
#15829=CARTESIAN_POINT('Ctrl Pts',(2.30761563827692,10.4994821320178,-32.899880823024));
#15830=CARTESIAN_POINT('Ctrl Pts',(2.34802797257454,10.4904368183652,-33.0135977355685));
#15831=CARTESIAN_POINT('Ctrl Pts',(2.47153733386496,10.4627922654998,-33.3611426987683));
#15832=CARTESIAN_POINT('Ctrl Pts',(2.59790667387361,10.4322221872737,-33.7074132218573));
#15833=CARTESIAN_POINT('Ctrl Pts',(2.72723242618058,10.3983029238487,-34.0520766794073));
#15834=CARTESIAN_POINT('Ctrl Pts',(2.73855742948338,10.3953326278058,-34.0822587175975));
#15835=CARTESIAN_POINT('Ctrl Pts',(2.74990510056545,10.3923366167857,-34.1124284238273));
#15836=CARTESIAN_POINT('Ctrl Pts',(2.76127550222649,10.3893145876333,-34.1425855701582));
#15837=CARTESIAN_POINT('Ctrl Pts',(2.82688668915726,10.3718764244496,-34.3166028321864));
#15838=CARTESIAN_POINT('Ctrl Pts',(2.89333478214233,10.353545519685,-34.4903953506847));
#15839=CARTESIAN_POINT('Ctrl Pts',(2.96045216056549,10.3343182822429,-34.6634673771716));
#15840=CARTESIAN_POINT('Ctrl Pts',(2.97372789147147,10.3305151594698,-34.6977008008388));
#15841=CARTESIAN_POINT('Ctrl Pts',(2.98702974707013,10.3266769758976,-34.7319058845362));
#15842=CARTESIAN_POINT('Ctrl Pts',(3.00035633927968,10.3228037152108,-34.7660785653831));
#15843=CARTESIAN_POINT('Ctrl Pts',(3.05923669243154,10.3056906413283,-34.9170623641498));
#15844=CARTESIAN_POINT('Ctrl Pts',(3.11875120969117,10.2878492854875,-35.067790011159));
#15845=CARTESIAN_POINT('Ctrl Pts',(3.17880504322561,10.2692598806997,-35.2179476948885));
#15846=CARTESIAN_POINT('Ctrl Pts',(3.26834234003258,10.2415439971999,-35.4418253777051));
#15847=CARTESIAN_POINT('Ctrl Pts',(3.35914405717775,10.2121611770426,-35.664696596617));
#15848=CARTESIAN_POINT('Ctrl Pts',(3.45130806413947,10.1809247273851,-35.8865571686193));
#15849=CARTESIAN_POINT('Ctrl Pts',(3.5428378271197,10.1499032372422,-36.1068909652874));
#15850=CARTESIAN_POINT('Ctrl Pts',(3.63571123956681,10.1170536586842,-36.32622788243));
#15851=CARTESIAN_POINT('Ctrl Pts',(3.7300172497872,10.0821701110365,-36.5445177725575));
#15852=CARTESIAN_POINT('Ctrl Pts',(3.82530348246398,10.0469239816542,-36.7650765811962));
#15853=CARTESIAN_POINT('Ctrl Pts',(3.92205232501441,10.009601592218,-36.9845664957216));
#15854=CARTESIAN_POINT('Ctrl Pts',(4.02034750426584,9.9699644333692,-37.2028890352372));
#15855=CARTESIAN_POINT('Ctrl Pts',(4.11864268351727,9.93032727452043,-37.4212115747528));
#15856=CARTESIAN_POINT('Ctrl Pts',(4.21848427264205,9.88837553750986,-37.6383666358546));
#15857=CARTESIAN_POINT('Ctrl Pts',(4.31994691208668,9.84384174532475,-37.8542100277662));
#15858=CARTESIAN_POINT('Ctrl Pts',(4.4053548532018,9.80635465134219,-38.0358999562699));
#15859=CARTESIAN_POINT('Ctrl Pts',(4.49191389406382,9.76703709863316,-38.2166288566652));
#15860=CARTESIAN_POINT('Ctrl Pts',(4.57972460013783,9.72568071370586,-38.3963878420291));
#15861=CARTESIAN_POINT('Ctrl Pts',(4.6608255353663,9.6874844430547,-38.5624111264386));
#15862=CARTESIAN_POINT('Ctrl Pts',(4.74299414110047,9.64754886738777,-38.7276065504812));
#15863=CARTESIAN_POINT('Ctrl Pts',(4.82630358598146,9.60569069335151,-38.8919330774156));
#15864=CARTESIAN_POINT('Ctrl Pts',(4.90218572876345,9.56756430872188,-39.0416093715923));
#15865=CARTESIAN_POINT('Ctrl Pts',(4.97901568325303,9.52783933124103,-39.1905324952375));
#15866=CARTESIAN_POINT('Ctrl Pts',(5.05684473081711,9.48635288415211,-39.3385881853721));
#15867=CARTESIAN_POINT('Ctrl Pts',(5.13087767175055,9.44688993576715,-39.4794224690444));
#15868=CARTESIAN_POINT('Ctrl Pts',(5.20580158441064,9.40584069224065,-39.6194691946357));
#15869=CARTESIAN_POINT('Ctrl Pts',(5.28171573049725,9.36301668766185,-39.7587113464906));
#15870=CARTESIAN_POINT('Ctrl Pts',(5.35632406157866,9.32092930768656,-39.8955583651507));
#15871=CARTESIAN_POINT('Ctrl Pts',(5.43188888911729,9.27712777578422,-40.0316282751385));
#15872=CARTESIAN_POINT('Ctrl Pts',(5.50849864130836,9.23141218451009,-40.1668597125731));
#15873=CARTESIAN_POINT('Ctrl Pts',(5.54813074309405,9.20776238908913,-40.2368182483959));
#15874=CARTESIAN_POINT('Ctrl Pts',(5.58804239379582,9.18359999168247,-40.3065516421872));
#15875=CARTESIAN_POINT('Ctrl Pts',(5.62824515816392,9.15889493550518,-40.3760464775971));
#15876=CARTESIAN_POINT('Ctrl Pts',(5.70446273045616,9.11205837004079,-40.5077968118102));
#15877=CARTESIAN_POINT('Ctrl Pts',(5.7817269628771,9.06327125490934,-40.6386852930296));
#15878=CARTESIAN_POINT('Ctrl Pts',(5.86011071648322,9.01230330186345,-40.7685536452058));
#15879=CARTESIAN_POINT('Ctrl Pts',(5.91380013799179,8.97739249715434,-40.8575077508697));
#15880=CARTESIAN_POINT('Ctrl Pts',(5.96788613468613,8.9415420249761,-40.9457714335191));
#15881=CARTESIAN_POINT('Ctrl Pts',(6.02244782126847,8.90464048909893,-41.0333877657161));
#15882=CARTESIAN_POINT('Ctrl Pts',(6.07897394762721,8.8664103497744,-41.1241586376426));
#15883=CARTESIAN_POINT('Ctrl Pts',(6.13590921669299,8.82711651296097,-41.2140642889579));
#15884=CARTESIAN_POINT('Ctrl Pts',(6.19324882975252,8.78670052824233,-41.3030092867015));
#15885=CARTESIAN_POINT('Ctrl Pts',(6.24844339663954,8.74779648524605,-41.3886268966795));
#15886=CARTESIAN_POINT('Ctrl Pts',(6.30401276283055,8.70785255316284,-41.4733544904255));
#15887=CARTESIAN_POINT('Ctrl Pts',(6.35993531577454,8.66681658635222,-41.5570616068614));
#15888=CARTESIAN_POINT('Ctrl Pts',(6.37627760299589,8.65482461673137,-41.5815233967342));
#15889=CARTESIAN_POINT('Ctrl Pts',(6.39264992778209,8.64273939541427,-41.6058977283417));
#15890=CARTESIAN_POINT('Ctrl Pts',(6.40905142809488,8.63055964540417,-41.6301805523135));
#15891=CARTESIAN_POINT('Ctrl Pts',(6.47123616750745,8.58438127354527,-41.7222465860356));
#15892=CARTESIAN_POINT('Ctrl Pts',(6.53391610435516,8.53680207855314,-41.8131519097231));
#15893=CARTESIAN_POINT('Ctrl Pts',(6.59715617547662,8.48765892211572,-41.9028104103885));
#15894=CARTESIAN_POINT('Ctrl Pts',(6.64315450335493,8.45191413273301,-41.9680244596069));
#15895=CARTESIAN_POINT('Ctrl Pts',(6.6894489682741,8.41534166165083,-42.0325779154381));
#15896=CARTESIAN_POINT('Ctrl Pts',(6.73606096464285,8.37787413518862,-42.0964212692311));
#15897=CARTESIAN_POINT('Ctrl Pts',(6.79685557701873,8.32900637741371,-42.1796902181925));
#15898=CARTESIAN_POINT('Ctrl Pts',(6.85815567161734,8.27864483486139,-42.261713048634));
#15899=CARTESIAN_POINT('Ctrl Pts',(6.92001935255261,8.22661679429675,-42.3423866349852));
#15900=CARTESIAN_POINT('Ctrl Pts',(6.98076429133924,8.17552962826482,-42.4216013210581));
#15901=CARTESIAN_POINT('Ctrl Pts',(7.04205264218131,8.12283573127723,-42.4995151699838));
#15902=CARTESIAN_POINT('Ctrl Pts',(7.10392919603158,8.06835766790845,-42.5759835345004));
#15903=CARTESIAN_POINT('Ctrl Pts',(7.13634361987152,8.03981899007116,-42.6160419705888));
#15904=CARTESIAN_POINT('Ctrl Pts',(7.16891928857766,8.01079045547862,-42.655702938709));
#15905=CARTESIAN_POINT('Ctrl Pts',(7.20166145050638,7.98124492776824,-42.6949402656682));
#15906=CARTESIAN_POINT('Ctrl Pts',(7.26062011125617,7.92804243158788,-42.7655947402859));
#15907=CARTESIAN_POINT('Ctrl Pts',(7.32024875525727,7.87304406856483,-42.8350315342943));
#15908=CARTESIAN_POINT('Ctrl Pts',(7.38032570976224,7.81630681970278,-42.9027542881581));
#15909=CARTESIAN_POINT('Ctrl Pts',(7.43888788904424,7.76100013900957,-42.9687694862639));
#15910=CARTESIAN_POINT('Ctrl Pts',(7.49787602412951,7.70404110584752,-43.0331559084488));
#15911=CARTESIAN_POINT('Ctrl Pts',(7.5570925960424,7.64549410734287,-43.0955009362299));
#15912=CARTESIAN_POINT('Ctrl Pts',(7.60084850666218,7.60223295339776,-43.1415685043963));
#15913=CARTESIAN_POINT('Ctrl Pts',(7.64472929783644,7.55810501350542,-43.1865224376846));
#15914=CARTESIAN_POINT('Ctrl Pts',(7.68865828488642,7.51314073311568,-43.2302138221615));
#15915=CARTESIAN_POINT('Ctrl Pts',(7.7355025987926,7.46519241910731,-43.2768047651101));
#15916=CARTESIAN_POINT('Ctrl Pts',(7.78245593008508,7.41623893382565,-43.3220139301323));
#15917=CARTESIAN_POINT('Ctrl Pts',(7.82953376245136,7.36619990654318,-43.3657719702781));
#15918=CARTESIAN_POINT('Ctrl Pts',(7.88858871032279,7.30343040337846,-43.4206625344753));
#15919=CARTESIAN_POINT('Ctrl Pts',(7.94783714305828,7.238948646025,-43.4732401474933));
#15920=CARTESIAN_POINT('Ctrl Pts',(8.00729466189754,7.172574346441,-43.5232677541047));
#15921=CARTESIAN_POINT('Ctrl Pts',(8.06675218073681,7.10620004685699,-43.5732953607162));
#15922=CARTESIAN_POINT('Ctrl Pts',(8.12641885383395,7.03793330216104,-43.6207732738916));
#15923=CARTESIAN_POINT('Ctrl Pts',(8.18629907590927,6.96757843036124,-43.6654106856205));
#15924=CARTESIAN_POINT('Ctrl Pts',(8.24126515839428,6.90299731238031,-43.7063848765967));
#15925=CARTESIAN_POINT('Ctrl Pts',(8.29641393605819,6.83664939573324,-43.744957765715));
#15926=CARTESIAN_POINT('Ctrl Pts',(8.35154990840288,6.76861619740753,-43.7807474995614));
#15927=CARTESIAN_POINT('Ctrl Pts',(8.38817263187795,6.72342680646271,-43.8045199564559));
#15928=CARTESIAN_POINT('Ctrl Pts',(8.42478989219045,6.67749412546476,-43.8270654294899));
#15929=CARTESIAN_POINT('Ctrl Pts',(8.46134684828429,6.63084530908934,-43.8482841545948));
#15930=CARTESIAN_POINT('Ctrl Pts',(8.51315982689053,6.56472891475219,-43.8783579207774));
#15931=CARTESIAN_POINT('Ctrl Pts',(8.56478254778382,6.49724643073336,-43.9056970713917));
#15932=CARTESIAN_POINT('Ctrl Pts',(8.61592734889603,6.42870112265509,-43.9300233884923));
#15933=CARTESIAN_POINT('Ctrl Pts',(8.63991916904507,6.39654679479161,-43.9414347658381));
#15934=CARTESIAN_POINT('Ctrl Pts',(8.66380578489985,6.36415902895718,-43.9521837717895));
#15935=CARTESIAN_POINT('Ctrl Pts',(8.6875574875569,6.33157122947104,-43.9622450359249));
#15936=CARTESIAN_POINT('Ctrl Pts',(8.7100395152484,6.30072544881139,-43.9717684634522));
#15937=CARTESIAN_POINT('Ctrl Pts',(8.73244740634613,6.26963643100526,-43.9806964803169));
#15938=CARTESIAN_POINT('Ctrl Pts',(8.75476238684806,6.23831993006402,-43.9890041654444));
#15939=CARTESIAN_POINT('Ctrl Pts',(8.81378476346905,6.15548883313143,-44.0109777145769));
#15940=CARTESIAN_POINT('Ctrl Pts',(8.87227654185962,6.07091644084457,-44.0286851829401));
#15941=CARTESIAN_POINT('Ctrl Pts',(8.93014977420605,5.98455779150124,-44.0417897287885));
#15942=CARTESIAN_POINT('Ctrl Pts',(8.96103257271427,5.93847436641886,-44.0487826861984));
#15943=CARTESIAN_POINT('Ctrl Pts',(8.99173501046401,5.89188620681016,-44.0544592798447));
#15944=CARTESIAN_POINT('Ctrl Pts',(9.02210965563433,5.84500106363286,-44.0587554593269));
#15945=CARTESIAN_POINT('Ctrl Pts',(9.02425298420913,5.841692703435,-44.0590586109915));
#15946=CARTESIAN_POINT('Ctrl Pts',(9.02639468638797,5.83838286767633,-44.0593549098961));
#15947=CARTESIAN_POINT('Ctrl Pts',(9.02853471298425,5.83507163079148,-44.0596443429017));
#15948=CARTESIAN_POINT('Ctrl Pts',(9.05887335222645,5.7881290266811,-44.0637475645889));
#15949=CARTESIAN_POINT('Ctrl Pts',(9.08887701332726,5.74090566265223,-44.066488459586));
#15950=CARTESIAN_POINT('Ctrl Pts',(9.11841089903929,5.6936166717973,-44.0678417494594));
#15951=CARTESIAN_POINT('Ctrl Pts',(9.13351347481917,5.66943476851156,-44.0685337736334));
#15952=CARTESIAN_POINT('Ctrl Pts',(9.14849342988732,5.64523582718803,-44.0688637450226));
#15953=CARTESIAN_POINT('Ctrl Pts',(9.16333413070452,5.62104938331967,-44.0688333130625));
#15954=CARTESIAN_POINT('Ctrl Pts',(9.27932019108639,5.43202257296252,-44.0685954750253));
#15955=CARTESIAN_POINT('Ctrl Pts',(9.38822404799286,5.24145243096134,-44.0465840027421));
#15956=CARTESIAN_POINT('Ctrl Pts',(9.49037895942472,5.04946426392216,-44.0034442094552));
#15957=CARTESIAN_POINT('Ctrl Pts',(9.52019775443346,4.99342333826522,-43.9908517982367));
#15958=CARTESIAN_POINT('Ctrl Pts',(9.54944152472417,4.93726132141394,-43.976459373685));
#15959=CARTESIAN_POINT('Ctrl Pts',(9.57811856097516,4.88098064194911,-43.9602834423684));
#15960=CARTESIAN_POINT('Ctrl Pts',(9.60473017663623,4.8287534941381,-43.9452725582802));
#15961=CARTESIAN_POINT('Ctrl Pts',(9.63080521238708,4.77651667385361,-43.9287441414905));
#15962=CARTESIAN_POINT('Ctrl Pts',(9.65625625560043,4.72448428046875,-43.9108030046278));
#15963=CARTESIAN_POINT('Ctrl Pts',(9.6818871281714,4.67208424196225,-43.8927351011296));
#15964=CARTESIAN_POINT('Ctrl Pts',(9.70688517903134,4.61989153984466,-43.873234453661));
#15965=CARTESIAN_POINT('Ctrl Pts',(9.73117419853334,4.5681320494209,-43.8524589796902));
#15966=CARTESIAN_POINT('Ctrl Pts',(9.74028176074149,4.54872398814212,-43.8446688784234));
#15967=CARTESIAN_POINT('Ctrl Pts',(9.74928976254928,4.5293769075458,-43.8367000449073));
#15968=CARTESIAN_POINT('Ctrl Pts',(9.7581946429713,4.51010296781278,-43.8285626112942));
#15969=CARTESIAN_POINT('Ctrl Pts',(9.79687625800233,4.4263795395857,-43.7932146830296));
#15970=CARTESIAN_POINT('Ctrl Pts',(9.83381278159481,4.34360625272283,-43.7545078688968));
#15971=CARTESIAN_POINT('Ctrl Pts',(9.86916355131065,4.26172191433118,-43.7127052462923));
#15972=CARTESIAN_POINT('Ctrl Pts',(9.88520563769071,4.22456301679624,-43.6937353260297));
#15973=CARTESIAN_POINT('Ctrl Pts',(9.90092094238594,4.18758710590883,-43.6741272004138));
#15974=CARTESIAN_POINT('Ctrl Pts',(9.91632327429603,4.15078809569389,-43.6539021212314));
#15975=CARTESIAN_POINT('Ctrl Pts',(9.92074536029067,4.14022291708081,-43.6480954005403));
#15976=CARTESIAN_POINT('Ctrl Pts',(9.92514262036429,4.12966998485364,-43.6422375099563));
#15977=CARTESIAN_POINT('Ctrl Pts',(9.92951515271414,4.11912962069325,-43.6363292143048));
#15978=CARTESIAN_POINT('Ctrl Pts',(9.96375695633186,4.03658681694431,-43.5900606716785));
#15979=CARTESIAN_POINT('Ctrl Pts',(9.99651370172761,3.95469685159093,-43.5405520961867));
#15980=CARTESIAN_POINT('Ctrl Pts',(10.0277460947657,3.87385088063219,-43.4883126423055));
#15981=CARTESIAN_POINT('Ctrl Pts',(10.0550083067909,3.80328184037399,-43.4427137326716));
#15982=CARTESIAN_POINT('Ctrl Pts',(10.0811094656132,3.73350767064565,-43.3950344467413));
#15983=CARTESIAN_POINT('Ctrl Pts',(10.106039106629,3.66476105295902,-43.3456209213272));
#15984=CARTESIAN_POINT('Ctrl Pts',(10.1302917164198,3.5978814339494,-43.2975493526476));
#15985=CARTESIAN_POINT('Ctrl Pts',(10.1534368297528,3.53198496973714,-43.2478594105363));
#15986=CARTESIAN_POINT('Ctrl Pts',(10.1755279180874,3.46715135906705,-43.1968184788605));
#15987=CARTESIAN_POINT('Ctrl Pts',(10.2029132663665,3.3867799902371,-43.1335452861024));
#15988=CARTESIAN_POINT('Ctrl Pts',(10.2287275666923,3.30790465592359,-43.0680938991004));
#15989=CARTESIAN_POINT('Ctrl Pts',(10.2531383414356,3.23042635812073,-43.0007320402055));
#15990=CARTESIAN_POINT('Ctrl Pts',(10.2557783158317,3.22204724174239,-42.993446995604));
#15991=CARTESIAN_POINT('Ctrl Pts',(10.2584018562662,3.21368446158842,-42.9861395596833));
#15992=CARTESIAN_POINT('Ctrl Pts',(10.2610091614446,3.20533788995049,-42.9788100374539));
#15993=CARTESIAN_POINT('Ctrl Pts',(10.2869627757754,3.12225451978362,-42.9058505715865));
#15994=CARTESIAN_POINT('Ctrl Pts',(10.3113115241219,3.04077434106045,-42.8307166031248));
#15995=CARTESIAN_POINT('Ctrl Pts',(10.3342333296949,2.96077179059331,-42.7536407000173));
#15996=CARTESIAN_POINT('Ctrl Pts',(10.3567452030436,2.88220000103875,-42.6779432178331));
#15997=CARTESIAN_POINT('Ctrl Pts',(10.3778805376574,2.80505340516852,-42.6003724329015));
#15998=CARTESIAN_POINT('Ctrl Pts',(10.3977881451373,2.72920873901186,-42.521098874524));
#15999=CARTESIAN_POINT('Ctrl Pts',(10.4182395169913,2.65129242122844,-42.4396600063825));
#16000=CARTESIAN_POINT('Ctrl Pts',(10.437395150398,2.57475010596009,-42.3564242397273));
#16001=CARTESIAN_POINT('Ctrl Pts',(10.4553967161795,2.4994440913569,-42.2715232305475));
#16002=CARTESIAN_POINT('Ctrl Pts',(10.4733982819609,2.42413807675371,-42.1866222213677));
#16003=CARTESIAN_POINT('Ctrl Pts',(10.4902456755578,2.35006832730552,-42.1000558923328));
#16004=CARTESIAN_POINT('Ctrl Pts',(10.5060622858798,2.27709359605912,-42.0119030752));
#16005=CARTESIAN_POINT('Ctrl Pts',(10.5060622858798,2.27709359605911,-42.0119030752));
#16006=CARTESIAN_POINT('Ctrl Pts',(10.5169067394724,2.22705941867769,-41.9514622401426));
#16007=CARTESIAN_POINT('Ctrl Pts',(10.5275633885531,2.1761749151871,-41.891851215819));
#16008=CARTESIAN_POINT('Ctrl Pts',(10.538021234015,2.12430565161473,-41.8331476931717));
#16009=CARTESIAN_POINT('Ctrl Pts',(10.5481140632636,2.0742468108728,-41.7764931334421));
#16010=CARTESIAN_POINT('Ctrl Pts',(10.5580217184636,2.02327075551396,-41.720683755564));
#16011=CARTESIAN_POINT('Ctrl Pts',(10.5677264286351,1.97125463207302,-41.6658361080088));
#16012=CARTESIAN_POINT('Ctrl Pts',(10.577366504854,1.91958493913805,-41.6113537490803));
#16013=CARTESIAN_POINT('Ctrl Pts',(10.5868063647818,1.86688899827979,-41.5578200279073));
#16014=CARTESIAN_POINT('Ctrl Pts',(10.596020405635,1.81304425509015,-41.5053993769448));
#16015=CARTESIAN_POINT('Ctrl Pts',(10.6089510763027,1.7374803789945,-41.4318340233089));
#16016=CARTESIAN_POINT('Ctrl Pts',(10.6214790124672,1.6594009572013,-41.3602207649006));
#16017=CARTESIAN_POINT('Ctrl Pts',(10.6334356950941,1.57886173480814,-41.2915861316767));
#16018=CARTESIAN_POINT('Ctrl Pts',(10.645584702412,1.49702702924925,-41.2218475020484));
#16019=CARTESIAN_POINT('Ctrl Pts',(10.6571438559943,1.41265274997818,-41.1551841633644));
#16020=CARTESIAN_POINT('Ctrl Pts',(10.6679353251557,1.32579537129823,-41.0927266082373));
#16021=CARTESIAN_POINT('Ctrl Pts',(10.6696041593524,1.3123634129981,-41.0830679322705));
#16022=CARTESIAN_POINT('Ctrl Pts',(10.6712546338859,1.29887206832203,-41.0735099376932));
#16023=CARTESIAN_POINT('Ctrl Pts',(10.6728860907067,1.28532154205633,-41.0640569152563));
#16024=CARTESIAN_POINT('Ctrl Pts',(10.6780427035461,1.24249183499117,-41.0341783574857));
#16025=CARTESIAN_POINT('Ctrl Pts',(10.683012291943,1.19904941834963,-41.0053284196112));
#16026=CARTESIAN_POINT('Ctrl Pts',(10.6877820649516,1.1549088847714,-40.9775991836193));
#16027=CARTESIAN_POINT('Ctrl Pts',(10.6931787645224,1.10496663423098,-40.9462252889483));
#16028=CARTESIAN_POINT('Ctrl Pts',(10.6983198661932,1.05413110185778,-40.9162884155456));
#16029=CARTESIAN_POINT('Ctrl Pts',(10.7031774103224,1.0022768629987,-40.8879610482626));
#16030=CARTESIAN_POINT('Ctrl Pts',(10.7079950829908,0.950848251617642,-40.859866196318));
#16031=CARTESIAN_POINT('Ctrl Pts',(10.7125338736272,0.898417599532796,-40.8333542553596));
#16032=CARTESIAN_POINT('Ctrl Pts',(10.7167580227179,0.844860405407882,-40.8086447312429));
#16033=CARTESIAN_POINT('Ctrl Pts',(10.7209821718086,0.791303211282969,-40.7839352071263));
#16034=CARTESIAN_POINT('Ctrl Pts',(10.7248917369913,0.736619490821813,-40.7610277021678));
#16035=CARTESIAN_POINT('Ctrl Pts',(10.7284416967453,0.680682389925007,-40.7401983449226));
#16036=CARTESIAN_POINT('Ctrl Pts',(10.7325618263942,0.6157610601505,-40.7160235208966));
#16037=CARTESIAN_POINT('Ctrl Pts',(10.7361457670398,0.549937828478586,-40.6949585895212));
#16038=CARTESIAN_POINT('Ctrl Pts',(10.7391417726632,0.483347761177844,-40.677326442336));
#16039=CARTESIAN_POINT('Ctrl Pts',(10.7420813231653,0.418012481349758,-40.6600265458647));
#16040=CARTESIAN_POINT('Ctrl Pts',(10.7444548707266,0.351938987296829,-40.6460314697351));
#16041=CARTESIAN_POINT('Ctrl Pts',(10.7462224401773,0.285256656119436,-40.635597438802));
#16042=CARTESIAN_POINT('Ctrl Pts',(10.7479495066408,0.220102317863198,-40.6254024985715));
#16043=CARTESIAN_POINT('Ctrl Pts',(10.7490980470938,0.154366722172408,-40.6186073686596));
#16044=CARTESIAN_POINT('Ctrl Pts',(10.7496394673345,0.0881723560645576,
-40.6154020700289));
#16045=CARTESIAN_POINT('Ctrl Pts',(10.7498716753067,0.0597824689281062,
-40.6140273598879));
#16046=CARTESIAN_POINT('Ctrl Pts',(10.7499923177763,0.0313082169392265,
-40.6133123467264));
#16047=CARTESIAN_POINT('Ctrl Pts',(10.7499996458547,0.0027593703269405,
-40.6132691037546));
#16048=CARTESIAN_POINT('Ctrl Pts',(10.749999802738,0.00214818153665405,
-40.6132681779862));
#16049=CARTESIAN_POINT('Ctrl Pts',(10.7499999071778,0.0015369585373491,
-40.6132675611916));
#16050=CARTESIAN_POINT('Ctrl Pts',(10.7499999591687,0.000925701661712846,
-40.613267253393));
#16051=CARTESIAN_POINT('Ctrl Pts',(10.7499999854151,0.000617123089545347,
-40.6132670980082));
#16052=CARTESIAN_POINT('Ctrl Pts',(10.7499999982932,0.000308555866768263,
-40.6132670215285));
#16053=CARTESIAN_POINT('Ctrl Pts',(10.7499999978076,2.23887749120318E-14,
-40.6132670239265));
#16054=CARTESIAN_POINT('Ctrl Pts',(1.18962879315414E-15,10.75,-25.));
#16055=CARTESIAN_POINT('Ctrl Pts',(1.18962879315414E-15,10.75,-25.));
#16056=CARTESIAN_POINT('Ctrl Pts',(1.18962879315414E-15,10.75,-25.));
#16057=CARTESIAN_POINT('Ctrl Pts',(-1.15016131432461,10.7499999999999,-25.006648030988));
#16058=CARTESIAN_POINT('Ctrl Pts',(-0.697561178987416,10.75,-25.5161421426786));
#16059=CARTESIAN_POINT('Ctrl Pts',(-0.245046068214511,10.75,-26.0262609450199));
#16060=CARTESIAN_POINT('Ctrl Pts',(-2.19083677072206,10.7494908638043,-24.9349427226934));
#16061=CARTESIAN_POINT('Ctrl Pts',(-1.34420969092897,10.7106820856761,-25.9683034993218));
#16062=CARTESIAN_POINT('Ctrl Pts',(-0.496527090382069,10.7416099797658,
-27.0012225209746));
#16063=CARTESIAN_POINT('Ctrl Pts',(-4.09261732542435,10.7476618345468,-24.7051472725922));
#16064=CARTESIAN_POINT('Ctrl Pts',(-2.54392000481286,10.5691405118102,-26.7758668839508));
#16065=CARTESIAN_POINT('Ctrl Pts',(-1.00994300948562,10.7055471241071,-28.8607675866442));
#16066=CARTESIAN_POINT('Ctrl Pts',(-4.95428344625941,10.7463421754083,-24.5465223290547));
#16067=CARTESIAN_POINT('Ctrl Pts',(-3.09790700297864,10.4667447449637,-27.1319561423712));
#16068=CARTESIAN_POINT('Ctrl Pts',(-1.27181081709599,10.6778869683601,-29.7457578698046));
#16069=CARTESIAN_POINT('Ctrl Pts',(-6.53601418471601,10.7430838699301,-24.1823266589109));
#16070=CARTESIAN_POINT('Ctrl Pts',(-4.12206177843065,10.2129395806112,-27.7692699064427));
#16071=CARTESIAN_POINT('Ctrl Pts',(-1.80395268087478,10.6009682382658,-31.4369952413258));
#16072=CARTESIAN_POINT('Ctrl Pts',(-7.25607013368073,10.7411450400571,-23.9764398761692));
#16073=CARTESIAN_POINT('Ctrl Pts',(-4.59251650314103,10.0612557981022,-28.0504746562229));
#16074=CARTESIAN_POINT('Ctrl Pts',(-2.07423302930113,10.5517189359563,-32.2432082848296));
#16075=CARTESIAN_POINT('Ctrl Pts',(-8.25213517452978,10.7379037306827,-23.6494263197586));
#16076=CARTESIAN_POINT('Ctrl Pts',(-5.23953949895351,9.8065491815586,-28.4251360768657));
#16077=CARTESIAN_POINT('Ctrl Pts',(-2.48491499500444,10.4597980983582,-33.398810870255));
#16078=CARTESIAN_POINT('Ctrl Pts',(-8.57010480087051,10.7367676447231,-23.5372843849539));
#16079=CARTESIAN_POINT('Ctrl Pts',(-5.44573262677527,9.71694384002046,-28.542284806436));
#16080=CARTESIAN_POINT('Ctrl Pts',(-2.62268926997625,10.4261480597686,-33.7750338413325));
#16081=CARTESIAN_POINT('Ctrl Pts',(-9.18102606498638,10.7344050046021,-23.30863371451));
#16082=CARTESIAN_POINT('Ctrl Pts',(-5.83934908124202,9.53003678683028,-28.7619697819756));
#16083=CARTESIAN_POINT('Ctrl Pts',(-2.89985851712548,10.3524819706059,-34.5101434304204));
#16084=CARTESIAN_POINT('Ctrl Pts',(-9.47464373380329,10.7331752085148,-23.191823577973));
#16085=CARTESIAN_POINT('Ctrl Pts',(-6.02717999588007,9.43244730398067,-28.8647092882211));
#16086=CARTESIAN_POINT('Ctrl Pts',(-3.03960350979001,10.312348987489,-34.8698754329709));
#16087=CARTESIAN_POINT('Ctrl Pts',(-10.8743639584978,10.7269099708188,-22.6058840900476));
#16088=CARTESIAN_POINT('Ctrl Pts',(-6.91554393551079,8.93206015782835,-29.3412703833179));
#16089=CARTESIAN_POINT('Ctrl Pts',(-3.73556853847291,10.0969166520402,-36.610324947681));
#16090=CARTESIAN_POINT('Ctrl Pts',(-11.786715064346,10.7215232478652,-22.1318450209703));
#16091=CARTESIAN_POINT('Ctrl Pts',(-7.45662740722064,8.49731281061401,-29.6013587996896));
#16092=CARTESIAN_POINT('Ctrl Pts',(-4.28614638191611,9.87708772192581,-37.8266979161691));
#16093=CARTESIAN_POINT('Ctrl Pts',(-12.9727671076994,10.7138050072996,-21.4442712536845));
#16094=CARTESIAN_POINT('Ctrl Pts',(-8.07505242268525,7.8660244748673,-29.8593172169878));
#16095=CARTESIAN_POINT('Ctrl Pts',(-5.09636724548306,9.46999968678062,-39.4245954567256));
#16096=CARTESIAN_POINT('Ctrl Pts',(-13.3368506180522,10.7112891987338,-21.218445186463));
#16097=CARTESIAN_POINT('Ctrl Pts',(-8.2491495137034,7.65808992648553,-29.922901554541));
#16098=CARTESIAN_POINT('Ctrl Pts',(-5.36385054816499,9.32136836042159,-39.9190359944887));
#16099=CARTESIAN_POINT('Ctrl Pts',(-13.8463351446538,10.7076931453776,-20.8854998552494));
#16100=CARTESIAN_POINT('Ctrl Pts',(-8.46819971826319,7.35863129856602,-29.9878091014236));
#16101=CARTESIAN_POINT('Ctrl Pts',(-5.76043976597223,9.07765988049979,-40.6045618673054));
#16102=CARTESIAN_POINT('Ctrl Pts',(-14.0100297822138,10.7065239150771,-20.7754673024019));
#16103=CARTESIAN_POINT('Ctrl Pts',(-8.53427798096343,7.26071615271009,-30.0043537934624));
#16104=CARTESIAN_POINT('Ctrl Pts',(-5.89186327262027,8.99295832117412,-40.8236913089009));
#16105=CARTESIAN_POINT('Ctrl Pts',(-14.326557040794,10.7042582843347,-20.5572849348335));
#16106=CARTESIAN_POINT('Ctrl Pts',(-8.65359144673208,7.07010518902838,-30.0276372056063));
#16107=CARTESIAN_POINT('Ctrl Pts',(-6.15303145469329,8.81632327601373,-41.2430881438711));
#16108=CARTESIAN_POINT('Ctrl Pts',(-14.478708980816,10.70316683247,-20.44959270127));
#16109=CARTESIAN_POINT('Ctrl Pts',(-8.70651740632404,6.97784314538739,-30.0342812550096));
#16110=CARTESIAN_POINT('Ctrl Pts',(-6.2822285175318,8.72473808032737,-41.4424366493996));
#16111=CARTESIAN_POINT('Ctrl Pts',(-15.2075066075735,10.6979795227471,-19.9216990174728));
#16112=CARTESIAN_POINT('Ctrl Pts',(-8.94085821143954,6.53572588791244,-30.0442270217656));
#16113=CARTESIAN_POINT('Ctrl Pts',(-6.9162933700514,8.25388281284964,-42.3814019788264));
#16114=CARTESIAN_POINT('Ctrl Pts',(-15.6958872062974,10.6946691527437,-19.5294610636527));
#16115=CARTESIAN_POINT('Ctrl Pts',(-9.02988049743652,6.24831397587878,-29.9786352046968));
#16116=CARTESIAN_POINT('Ctrl Pts',(-7.39039954503943,7.83295516260822,-42.9577462277717));
#16117=CARTESIAN_POINT('Ctrl Pts',(-16.3468106290142,10.691138463815,-18.9727916173314));
#16118=CARTESIAN_POINT('Ctrl Pts',(-9.10237201213877,5.93389687773062,-29.7948677586647));
#16119=CARTESIAN_POINT('Ctrl Pts',(-8.04909500484054,7.13282851376216,-43.5698483134323));
#16120=CARTESIAN_POINT('Ctrl Pts',(-16.5497974875563,10.6901975107843,-18.7924848319928));
#16121=CARTESIAN_POINT('Ctrl Pts',(-9.11615528018351,5.84830420961477,-29.7188377297072));
#16122=CARTESIAN_POINT('Ctrl Pts',(-8.25987706424781,6.88793250317559,-43.7313745857345));
#16123=CARTESIAN_POINT('Ctrl Pts',(-16.838428413657,10.6891335560231,-18.527932522204));
#16124=CARTESIAN_POINT('Ctrl Pts',(-9.13155934276341,5.74903975065829,-29.5835434645598));
#16125=CARTESIAN_POINT('Ctrl Pts',(-8.56208087001509,6.50230282257902,-43.9067575462197));
#16126=CARTESIAN_POINT('Ctrl Pts',(-16.931739932865,10.688837856098,-18.4409474186566));
#16127=CARTESIAN_POINT('Ctrl Pts',(-9.13580403755556,5.72089613947525,-29.5349142032813));
#16128=CARTESIAN_POINT('Ctrl Pts',(-8.66022380779681,6.37099391565298,-43.9538118068058));
#16129=CARTESIAN_POINT('Ctrl Pts',(-17.1115634445619,10.6883619233172,-18.270761756668));
#16130=CARTESIAN_POINT('Ctrl Pts',(-9.14417010468671,5.67448452401008,-29.4318726265361));
#16131=CARTESIAN_POINT('Ctrl Pts',(-8.84930077011382,6.10564621923683,-44.0242038964093));
#16132=CARTESIAN_POINT('Ctrl Pts',(-17.1983679656057,10.6881805558801,-18.1872937563323));
#16133=CARTESIAN_POINT('Ctrl Pts',(-9.14830611568215,5.65612786905982,-29.3773294151916));
#16134=CARTESIAN_POINT('Ctrl Pts',(-8.94054219798206,5.97122136470856,-44.0477302440176));
#16135=CARTESIAN_POINT('Ctrl Pts',(-17.6191726876552,10.6875284847955,-17.7768657002981));
#16136=CARTESIAN_POINT('Ctrl Pts',(-9.17281269728736,5.58625383845738,-29.0892695495114));
#16137=CARTESIAN_POINT('Ctrl Pts',(-9.38050433358122,5.29047337500718,-44.1073526930303));
#16138=CARTESIAN_POINT('Ctrl Pts',(-17.9141135504146,10.6878308215939,-17.4708062072169));
#16139=CARTESIAN_POINT('Ctrl Pts',(-9.20577389365999,5.60207456542975,-28.8138270066121));
#16140=CARTESIAN_POINT('Ctrl Pts',(-9.68088377276871,4.71847711576912,-43.9723394445427));
#16141=CARTESIAN_POINT('Ctrl Pts',(-18.2589538640075,10.6887007240517,-17.0967280701274));
#16142=CARTESIAN_POINT('Ctrl Pts',(-9.31430913574479,5.66760812797665,-28.3986430019926));
#16143=CARTESIAN_POINT('Ctrl Pts',(-9.99167371036611,3.96929102897446,-43.5523436135201));
#16144=CARTESIAN_POINT('Ctrl Pts',(-18.3268647339594,10.6888993216382,-17.0221379112497));
#16145=CARTESIAN_POINT('Ctrl Pts',(-9.33939465884606,5.68300852364718,-28.3116880707622));
#16146=CARTESIAN_POINT('Ctrl Pts',(-10.0507078465264,3.8173439659334,-43.4552961639041));
#16147=CARTESIAN_POINT('Ctrl Pts',(-18.4599063361282,10.6893257513556,-16.8742773574252));
#16148=CARTESIAN_POINT('Ctrl Pts',(-9.39669476979905,5.71674608902978,-28.130888942994));
#16149=CARTESIAN_POINT('Ctrl Pts',(-10.1613705280412,3.51217769515325,-43.2359489845917));
#16150=CARTESIAN_POINT('Ctrl Pts',(-18.525020225263,10.6895533451493,-16.801031713128));
#16151=CARTESIAN_POINT('Ctrl Pts',(-9.42887151311381,5.73505897199891,-28.0371197976092));
#16152=CARTESIAN_POINT('Ctrl Pts',(-10.2130004334533,3.35902467638586,-43.1137730065137));
#16153=CARTESIAN_POINT('Ctrl Pts',(-18.7174485368953,10.6902545953255,-16.5820822167333));
#16154=CARTESIAN_POINT('Ctrl Pts',(-9.53687563692295,5.79224969484422,-27.7441005175946));
#16155=CARTESIAN_POINT('Ctrl Pts',(-10.3572302487592,2.89731244717209,-42.708321547074));
#16156=CARTESIAN_POINT('Ctrl Pts',(-18.8415676478173,10.6907456279116,-16.43750807407));
#16157=CARTESIAN_POINT('Ctrl Pts',(-9.62413492807353,5.83327722471964,-27.5336716867507));
#16158=CARTESIAN_POINT('Ctrl Pts',(-10.4389331022223,2.58709663538484,-42.3866080951754));
#16159=CARTESIAN_POINT('Ctrl Pts',(-18.9640555125017,10.6911940224261,-16.2915944549513));
#16160=CARTESIAN_POINT('Ctrl Pts',(-9.72768081900659,5.87165951671932,-27.3036545666179));
#16161=CARTESIAN_POINT('Ctrl Pts',(-10.5064904280787,2.27511733549709,-42.0095150580924));
#16162=CARTESIAN_POINT('',(-17.2858341932293,9.77439024390244,-18.4545876051761));
#16163=CARTESIAN_POINT('Origin',(-49.598387070549,10.75,-42.0119030752));
#16164=CARTESIAN_POINT('Ctrl Pts',(-17.2858341932293,9.77439024390244,-18.4545876051761));
#16165=CARTESIAN_POINT('Ctrl Pts',(-17.230849614275,9.81433280796118,-18.5283533855738));
#16166=CARTESIAN_POINT('Ctrl Pts',(-17.1734819746949,9.85746553470479,-18.598137817752));
#16167=CARTESIAN_POINT('Ctrl Pts',(-17.0519080073572,9.93927316613436,-18.7329980624538));
#16168=CARTESIAN_POINT('Ctrl Pts',(-16.9877799937368,9.97756355387077,-18.7983427112246));
#16169=CARTESIAN_POINT('Ctrl Pts',(-16.7876064605023,10.0797362530432,-18.9927736277449));
#16170=CARTESIAN_POINT('Ctrl Pts',(-16.644430688312,10.1320778149371,-19.1203515704376));
#16171=CARTESIAN_POINT('Ctrl Pts',(-16.200446986055,10.2641590938576,-19.5007895704327));
#16172=CARTESIAN_POINT('Ctrl Pts',(-15.8905894180578,10.3204314322063,-19.7454341656197));
#16173=CARTESIAN_POINT('Ctrl Pts',(-14.9458920693911,10.4612218351731,-20.4514044399693));
#16174=CARTESIAN_POINT('Ctrl Pts',(-14.2895068016006,10.5142230477087,-20.8884604785083));
#16175=CARTESIAN_POINT('Ctrl Pts',(-12.9348288042002,10.5988273843319,-21.7028449453777));
#16176=CARTESIAN_POINT('Ctrl Pts',(-12.2340573634712,10.6275795411286,-22.0806151123365));
#16177=CARTESIAN_POINT('Ctrl Pts',(-10.8051035470393,10.672309925593,-22.7688021724106));
#16178=CARTESIAN_POINT('Ctrl Pts',(-10.0759536654712,10.6880415610146,-23.0799285438411));
#16179=CARTESIAN_POINT('Ctrl Pts',(-7.84464084215434,10.7247738680017,-23.9142122954436));
#16180=CARTESIAN_POINT('Ctrl Pts',(-6.30784220188913,10.7354998258494,-24.3342560266836));
#16181=CARTESIAN_POINT('Ctrl Pts',(-3.96162521204357,10.7451589131064,-24.7482204101398));
#16182=CARTESIAN_POINT('Ctrl Pts',(-3.1741229733078,10.7471212251943,-24.8500338800463));
#16183=CARTESIAN_POINT('Ctrl Pts',(-1.98574081627447,10.7489410804811,-24.9478353565518));
#16184=CARTESIAN_POINT('Ctrl Pts',(-1.58913075295951,10.749354887983,-24.9712158778548));
#16185=CARTESIAN_POINT('Ctrl Pts',(-0.794943421248679,10.7498845226873,
-24.9995000067156));
#16186=CARTESIAN_POINT('Ctrl Pts',(-0.396138629816618,10.75,-25.0040317725612));
#16187=CARTESIAN_POINT('Ctrl Pts',(4.08240831242321E-16,10.75,-25.));
#16188=CARTESIAN_POINT('Ctrl Pts',(-19.0763027194419,10.75,-16.1584242596923));
#16189=CARTESIAN_POINT('Ctrl Pts',(-9.72158531033335,5.89651617104406,-27.202410868965));
#16190=CARTESIAN_POINT('Ctrl Pts',(-10.5060622858798,2.27709359605911,-42.0119030752));
#16191=CARTESIAN_POINT('Ctrl Pts',(-19.2216718028992,9.00616861666823,-15.9868045152475));
#16192=CARTESIAN_POINT('Ctrl Pts',(-10.054211023792,4.97457944704813,-27.0105294870454));
#16193=CARTESIAN_POINT('Ctrl Pts',(-10.5861279548367,1.90768633652585,-41.5656624370341));
#16194=CARTESIAN_POINT('Ctrl Pts',(-19.3319171300942,7.24098469274974,-15.8521571440323));
#16195=CARTESIAN_POINT('Ctrl Pts',(-10.3116563320604,4.01333959595937,-26.8528714213347));
#16196=CARTESIAN_POINT('Ctrl Pts',(-10.6468390893589,1.53380463935034,-41.2156085744383));
#16197=CARTESIAN_POINT('Ctrl Pts',(-19.4806014076805,3.66349219259715,-15.6690802167518));
#16198=CARTESIAN_POINT('Ctrl Pts',(-10.6587854631624,2.04350040512538,-26.6371988427526));
#16199=CARTESIAN_POINT('Ctrl Pts',(-10.7287253073072,0.776010661486689,
-40.7396085636003));
#16200=CARTESIAN_POINT('Ctrl Pts',(-19.5190486552012,1.85116909998969,-15.6207150822312));
#16201=CARTESIAN_POINT('Ctrl Pts',(-10.7495724464151,1.0318365325806,-26.578717448758));
#16202=CARTESIAN_POINT('Ctrl Pts',(-10.7498997026982,0.392119563051999,
-40.6138592138001));
#16203=CARTESIAN_POINT('Ctrl Pts',(-19.5192754939424,-0.446508782486855,
-15.6204316264581));
#16204=CARTESIAN_POINT('Ctrl Pts',(-10.75010500077,-0.248881490684448,-26.5783781675765));
#16205=CARTESIAN_POINT('Ctrl Pts',(-10.7500246316438,-0.0945806780637169,
-40.6131222287912));
#16206=CARTESIAN_POINT('Ctrl Pts',(-19.5169052717251,-0.907660808398219,
-15.6233948374126));
#16207=CARTESIAN_POINT('Ctrl Pts',(-10.7445382243028,-0.505954113601866,
-26.5819274926781));
#16208=CARTESIAN_POINT('Ctrl Pts',(-10.7487192580301,-0.192263126902217,
-40.6208265772774));
#16209=CARTESIAN_POINT('Ctrl Pts',(-19.507413247859,-1.82424936484475,-15.6352449935534));
#16210=CARTESIAN_POINT('Ctrl Pts',(-10.7222613599582,-1.01646923646727,
-26.5960974937392));
#16211=CARTESIAN_POINT('Ctrl Pts',(-10.7434916310807,-0.386417353144324,
-40.6516369832341));
#16212=CARTESIAN_POINT('Ctrl Pts',(-19.5002954912967,-2.28081367063997,
-15.6441267958189));
#16213=CARTESIAN_POINT('Ctrl Pts',(-10.705556116365,-1.27059431610894,-26.6067148813092));
#16214=CARTESIAN_POINT('Ctrl Pts',(-10.7395716055577,-0.483128018904318,
-40.6747296691341));
#16215=CARTESIAN_POINT('Ctrl Pts',(-19.4719617901058,-3.64544085441919,
-15.6794009404326));
#16216=CARTESIAN_POINT('Ctrl Pts',(-10.6391149691374,-2.02907825197536,
-26.6487780897149));
#16217=CARTESIAN_POINT('Ctrl Pts',(-10.7239671336519,-0.772186979014334,
-40.7664424451148));
#16218=CARTESIAN_POINT('Ctrl Pts',(-19.4437719857229,-4.54843815679108,
-15.7144269835628));
#16219=CARTESIAN_POINT('Ctrl Pts',(-10.5730189889065,-2.52952302522724,
-26.6904822440918));
#16220=CARTESIAN_POINT('Ctrl Pts',(-10.708441911361,-0.963462269665953,
-40.8575101572862));
#16221=CARTESIAN_POINT('Ctrl Pts',(-19.3321340685403,-7.23816397108207,
-15.851893583229));
#16222=CARTESIAN_POINT('Ctrl Pts',(-10.3121595644709,-4.01182480387595,
-26.8525659713277));
#16223=CARTESIAN_POINT('Ctrl Pts',(-10.6469585658025,-1.53320714658219,
-41.2149233163493));
#16224=CARTESIAN_POINT('Ctrl Pts',(-19.221715988843,-9.00563856695385,-15.9867523502327));
#16225=CARTESIAN_POINT('Ctrl Pts',(-10.0543097325788,-4.97430585631275,
-27.0104725449986));
#16226=CARTESIAN_POINT('Ctrl Pts',(-10.5861513134396,-1.90757856452286,
-41.5655322494524));
#16227=CARTESIAN_POINT('Ctrl Pts',(-19.0763027194419,-10.75,-16.1584242596923));
#16228=CARTESIAN_POINT('Ctrl Pts',(-9.72158531033335,-5.89651617104406,
-27.202410868965));
#16229=CARTESIAN_POINT('Ctrl Pts',(-10.5060622858798,-2.27709359605911,
-42.0119030752));
#16230=CARTESIAN_POINT('',(-17.2858341932293,-9.77439024390244,-18.4545876051761));
#16231=CARTESIAN_POINT('Origin',(-49.598387070549,-10.75,-42.0119030752));
#16232=CARTESIAN_POINT('Origin',(-58.1890816870435,-11.0623060839995,-60.5701599251957));
#16233=CARTESIAN_POINT('Origin',(-58.6872612779838,11.078510305597,-61.1099570363713));
#16234=CARTESIAN_POINT('Ctrl Pts',(2.51461494246785E-15,-10.75,-25.));
#16235=CARTESIAN_POINT('Ctrl Pts',(2.51461494246785E-15,-10.75,-25.));
#16236=CARTESIAN_POINT('Ctrl Pts',(2.51461494246785E-15,-10.75,-25.));
#16237=CARTESIAN_POINT('Ctrl Pts',(-0.245046068214529,-10.75,-26.02626094502));
#16238=CARTESIAN_POINT('Ctrl Pts',(-0.697525526200558,-10.7499999999999,
-25.5161823339491));
#16239=CARTESIAN_POINT('Ctrl Pts',(-1.15008999541957,-10.7499999999998,
-25.006728315021));
#16240=CARTESIAN_POINT('Ctrl Pts',(-0.496527090381411,-10.7416099797658,
-27.0012225209746));
#16241=CARTESIAN_POINT('Ctrl Pts',(-1.34414287446072,-10.7106845234903,
-25.9683849165885));
#16242=CARTESIAN_POINT('Ctrl Pts',(-2.19070342017083,-10.7494847515439,
-24.9351054852879));
#16243=CARTESIAN_POINT('Ctrl Pts',(-1.00994300948628,-10.7055471241071,
-28.8607675866442));
#16244=CARTESIAN_POINT('Ctrl Pts',(-2.54379890564962,-10.5691512803725,
-26.7760314755534));
#16245=CARTESIAN_POINT('Ctrl Pts',(-4.09237376553143,-10.7476337608733,
-24.7054729298822));
#16246=CARTESIAN_POINT('Ctrl Pts',(-1.27181081710183,-10.6778869683592,
-29.7457578698046));
#16247=CARTESIAN_POINT('Ctrl Pts',(-3.09776268237128,-10.4667614320226,
-27.1321627171777));
#16248=CARTESIAN_POINT('Ctrl Pts',(-4.95399181836562,-10.7462982550018,
-24.5469284888288));
#16249=CARTESIAN_POINT('Ctrl Pts',(-1.80395268086896,-10.6009682382667,
-31.4369952413258));
#16250=CARTESIAN_POINT('Ctrl Pts',(-4.1218780716154,-10.2129703313243,-27.7695605683977));
#16251=CARTESIAN_POINT('Ctrl Pts',(-6.53563598592608,-10.7430008167255,
-24.1828886339226));
#16252=CARTESIAN_POINT('Ctrl Pts',(-2.0742330292986,-10.5517189359568,-32.2432082848296));
#16253=CARTESIAN_POINT('Ctrl Pts',(-4.59231660856942,-10.0612947297469,
-28.0508074641415));
#16254=CARTESIAN_POINT('Ctrl Pts',(-7.25565349765545,-10.74103869806,-23.9770771433437));
#16255=CARTESIAN_POINT('Ctrl Pts',(-2.48491499500571,-10.4597980983579,
-33.398810870255));
#16256=CARTESIAN_POINT('Ctrl Pts',(-5.23932024815341,-9.80660117606759,
-28.4255319501264));
#16257=CARTESIAN_POINT('Ctrl Pts',(-8.25166520613066,-10.7377584476419,
-23.6501713397551));
#16258=CARTESIAN_POINT('Ctrl Pts',(-2.62268926997313,-10.4261480597694,
-33.7750338413325));
#16259=CARTESIAN_POINT('Ctrl Pts',(-5.44550771521678,-9.71700034224351,
-28.5427016989824));
#16260=CARTESIAN_POINT('Ctrl Pts',(-8.56961785539663,-10.7366087113668,
-23.5380644380174));
#16261=CARTESIAN_POINT('Ctrl Pts',(-2.8998585171286,-10.352481970605,-34.5101434304204));
#16262=CARTESIAN_POINT('Ctrl Pts',(-5.83911442424541,-9.53010244192036,
-28.7624286537232));
#16263=CARTESIAN_POINT('Ctrl Pts',(-9.18050627770339,-10.7342176806201,
-23.3094819695874));
#16264=CARTESIAN_POINT('Ctrl Pts',(-3.03960350979062,-10.3123489874888,
-34.8698754329709));
#16265=CARTESIAN_POINT('Ctrl Pts',(-6.02694125129918,-9.43251761908732,
-28.8651891758106));
#16266=CARTESIAN_POINT('Ctrl Pts',(-9.47410804388434,-10.7329731051953,
-23.1927050755687));
#16267=CARTESIAN_POINT('Ctrl Pts',(-3.73556853847047,-10.096916652041,-36.610324947681));
#16268=CARTESIAN_POINT('Ctrl Pts',(-6.91528845193507,-8.93215374399242,
-29.3418543891044));
#16269=CARTESIAN_POINT('Ctrl Pts',(-10.8737520539574,-10.7266325617244,
-22.6069251727742));
#16270=CARTESIAN_POINT('Ctrl Pts',(-4.28614638192033,-9.87708772192369,
-37.8266979161691));
#16271=CARTESIAN_POINT('Ctrl Pts',(-7.45637148838566,-8.49742418500439,
-29.6020227428502));
#16272=CARTESIAN_POINT('Ctrl Pts',(-11.7860488689348,-10.7211810659044,
-22.1329942424813));
#16273=CARTESIAN_POINT('Ctrl Pts',(-5.09636724548095,-9.46999968678168,
-39.4245954567256));
#16274=CARTESIAN_POINT('Ctrl Pts',(-8.07481027122082,-7.86615486962916,
-29.8600948238844));
#16275=CARTESIAN_POINT('Ctrl Pts',(-12.9720188517199,-10.7133699539135,
-21.4455569030438));
#16276=CARTESIAN_POINT('Ctrl Pts',(-5.36385054816499,-9.32136836042159,
-39.9190359944887));
#16277=CARTESIAN_POINT('Ctrl Pts',(-8.24891439361641,-7.65822546536235,
-29.923716129418));
#16278=CARTESIAN_POINT('Ctrl Pts',(-13.336075167167,-10.7108238610927,-21.2197719228705));
#16279=CARTESIAN_POINT('Ctrl Pts',(-5.76043976597223,-9.07765988049979,
-40.6045618673054));
#16280=CARTESIAN_POINT('Ctrl Pts',(-8.46797828136676,-7.35877187836447,
-29.9886773248984));
#16281=CARTESIAN_POINT('Ctrl Pts',(-13.8455182954065,-10.7071844997807,
-20.8868823819796));
#16282=CARTESIAN_POINT('Ctrl Pts',(-5.89186327261934,-8.99295832117475,
-40.8236913089009));
#16283=CARTESIAN_POINT('Ctrl Pts',(-8.53406163310364,-7.26085798014581,
-30.0052396273611));
#16284=CARTESIAN_POINT('Ctrl Pts',(-14.0091990745616,-10.7060011844055,
-20.776867424868));
#16285=CARTESIAN_POINT('Ctrl Pts',(-6.15303145469421,-8.81632327601311,
-41.2430881438711));
#16286=CARTESIAN_POINT('Ctrl Pts',(-8.65338623383247,-7.07024849551272,
-30.0285576215158));
#16287=CARTESIAN_POINT('Ctrl Pts',(-14.3256984012058,-10.7037082528389,
-20.5587183768881));
#16288=CARTESIAN_POINT('Ctrl Pts',(-6.28222851753179,-8.72473808032737,
-41.4424366493996));
#16289=CARTESIAN_POINT('Ctrl Pts',(-8.70631822275726,-6.97798667315792,
-30.0352185678562));
#16290=CARTESIAN_POINT('Ctrl Pts',(-14.4778363196157,-10.7026036448698,
-20.4510417956705));
#16291=CARTESIAN_POINT('Ctrl Pts',(-6.91629337005139,-8.25388281284964,
-42.3814019788264));
#16292=CARTESIAN_POINT('Ctrl Pts',(-8.94069092645878,-6.5358678551081,-30.0452464131274));
#16293=CARTESIAN_POINT('Ctrl Pts',(-15.2065644724196,-10.6973537837553,
-19.9232209063353));
#16294=CARTESIAN_POINT('Ctrl Pts',(-7.39039954503927,-7.83295516260838,
-42.9577462277717));
#16295=CARTESIAN_POINT('Ctrl Pts',(-9.02974446998217,-6.24844545337749,
-29.9797120796148));
#16296=CARTESIAN_POINT('Ctrl Pts',(-15.6948891167241,-10.6940034243733,
-19.5310256649458));
#16297=CARTESIAN_POINT('Ctrl Pts',(-8.04909500484061,-7.13282851376207,
-43.5698483134323));
#16298=CARTESIAN_POINT('Ctrl Pts',(-9.10228415266927,-5.93399688698298,
-29.7960168032289));
#16299=CARTESIAN_POINT('Ctrl Pts',(-16.345731657509,-10.6904299419629,-18.9744035104728));
#16300=CARTESIAN_POINT('Ctrl Pts',(-8.25987706425041,-6.88793250317227,
-43.7313745857345));
#16301=CARTESIAN_POINT('Ctrl Pts',(-9.1160837358347,-5.84839107335997,-29.7200085149803));
#16302=CARTESIAN_POINT('Ctrl Pts',(-16.5486921356379,-10.6894775511536,
-18.7941096148084));
#16303=CARTESIAN_POINT('Ctrl Pts',(-8.56208087001378,-6.50230282258068,
-43.9067575462197));
#16304=CARTESIAN_POINT('Ctrl Pts',(-9.13151165542614,-5.74910282786052,
-29.5847428705483));
#16305=CARTESIAN_POINT('Ctrl Pts',(-16.8372849488646,-10.6884006034147,
-18.529572922268));
#16306=CARTESIAN_POINT('Ctrl Pts',(-8.66022380779591,-6.37099391565426,
-43.9538118068058));
#16307=CARTESIAN_POINT('Ctrl Pts',(-9.13576418532011,-5.72095061576736,
-29.5361224647812));
#16308=CARTESIAN_POINT('Ctrl Pts',(-16.9305840510713,-10.6881012790773,
-18.4425923757168));
#16309=CARTESIAN_POINT('Ctrl Pts',(-8.84930077011471,-6.10564621923558,
-44.0242038964093));
#16310=CARTESIAN_POINT('Ctrl Pts',(-9.1441453635236,-5.67452070085838,-29.4330970036618));
#16311=CARTESIAN_POINT('Ctrl Pts',(-17.1103836503878,-10.687619483155,-18.2724145576342));
#16312=CARTESIAN_POINT('Ctrl Pts',(-8.94054219798145,-5.9712213647095,-44.0477302440176));
#16313=CARTESIAN_POINT('Ctrl Pts',(-9.14828867272208,-5.6561543229398,-29.3785610783257));
#16314=CARTESIAN_POINT('Ctrl Pts',(-17.1971766337535,-10.6874358631681,
-18.1889498635026));
#16315=CARTESIAN_POINT('Ctrl Pts',(-9.38050433358363,-5.29047337500344,
-44.1073526930303));
#16316=CARTESIAN_POINT('Ctrl Pts',(-9.17283018205915,-5.58622893784892,
-29.0905338638653));
#16317=CARTESIAN_POINT('Ctrl Pts',(-17.617926090303,-10.6867755856068,-17.7785353917849));
#16318=CARTESIAN_POINT('Ctrl Pts',(-9.68088377276682,-4.71847711577368,
-43.9723394445427));
#16319=CARTESIAN_POINT('Ctrl Pts',(-9.20581394722617,-5.60200007483861,
-28.8151049264038));
#16320=CARTESIAN_POINT('Ctrl Pts',(-17.9128300606806,-10.6870812437168,
-17.4724781108102));
#16321=CARTESIAN_POINT('Ctrl Pts',(-9.99167371036658,-3.96929102897332,
-43.5523436135201));
#16322=CARTESIAN_POINT('Ctrl Pts',(-9.31436628119189,-5.66746485048706,
-28.3999214347156));
#16323=CARTESIAN_POINT('Ctrl Pts',(-18.2576364829922,-10.6879611969071,
-17.0983927329858));
#16324=CARTESIAN_POINT('Ctrl Pts',(-10.0507078465267,-3.81734396593254,
-43.4552961639041));
#16325=CARTESIAN_POINT('Ctrl Pts',(-9.33945467389634,-5.68285111346893,
-28.3129657699404));
#16326=CARTESIAN_POINT('Ctrl Pts',(-18.3255411664155,-10.6881620996133,
-17.0238006013664));
#16327=CARTESIAN_POINT('Ctrl Pts',(-10.1613705280408,-3.51217769515411,
-43.2359489845917));
#16328=CARTESIAN_POINT('Ctrl Pts',(-9.39675929232103,-5.71656006988305,
-28.1321634919568));
#16329=CARTESIAN_POINT('Ctrl Pts',(-18.4585717202441,-10.6885934908853,
-16.8759350652419));
#16330=CARTESIAN_POINT('Ctrl Pts',(-10.2130004334533,-3.35902467638586,
-43.1137730065137));
#16331=CARTESIAN_POINT('Ctrl Pts',(-9.42893767629744,-5.73485848711403,
-28.0383919345897));
#16332=CARTESIAN_POINT('Ctrl Pts',(-18.5236807436346,-10.6888237382775,
-16.8026864178631));
#16333=CARTESIAN_POINT('Ctrl Pts',(-10.3585730211466,-2.89301392934481,
-42.7045468142075));
#16334=CARTESIAN_POINT('Ctrl Pts',(-9.53795019632931,-5.79253740708886,
-27.7426353598479));
#16335=CARTESIAN_POINT('Ctrl Pts',(-18.7178877505159,-10.6895397759366,
-16.5816878126578));
#16336=CARTESIAN_POINT('Ctrl Pts',(-10.4412106172238,-2.57843802588067,
-42.3776190357652));
#16337=CARTESIAN_POINT('Ctrl Pts',(-9.62664120342293,-5.83414789935946,
-27.529049966199));
#16338=CARTESIAN_POINT('Ctrl Pts',(-18.8436728020004,-10.6900438114354,
-16.4351079573943));
#16339=CARTESIAN_POINT('Ctrl Pts',(-10.509310471686,-2.26205520316976,-41.9936955835997));
#16340=CARTESIAN_POINT('Ctrl Pts',(-9.73208854795376,-5.87295961154644,
-27.2952574763174));
#16341=CARTESIAN_POINT('Ctrl Pts',(-18.9678208706686,-10.690502528869,-16.2871078568861));
#16342=CARTESIAN_POINT('Ctrl Pts',(0.,-10.75,-25.));
#16343=CARTESIAN_POINT('Ctrl Pts',(-1.58979632319829,-10.75,-25.0161723660006));
#16344=CARTESIAN_POINT('Ctrl Pts',(-3.17967643758472,-10.7483783455921,
-24.8861937318557));
#16345=CARTESIAN_POINT('Ctrl Pts',(-6.30793928508339,-10.7354991807564,
-24.3342319030052));
#16346=CARTESIAN_POINT('Ctrl Pts',(-7.8447242833345,-10.7247729855381,-23.9141859389712));
#16347=CARTESIAN_POINT('Ctrl Pts',(-10.0760168613864,-10.6880402750731,
-23.0799024938186));
#16348=CARTESIAN_POINT('Ctrl Pts',(-10.8051602308081,-10.6723084956847,
-22.768776762151));
#16349=CARTESIAN_POINT('Ctrl Pts',(-12.2341014639979,-10.6275778161729,
-22.0805919845415));
#16350=CARTESIAN_POINT('Ctrl Pts',(-12.9348666409598,-10.5988255131215,
-21.7028235613396));
#16351=CARTESIAN_POINT('Ctrl Pts',(-14.289532661915,-10.5142209407928,-20.8884435700559));
#16352=CARTESIAN_POINT('Ctrl Pts',(-14.9459122468717,-10.461219629094,-20.4513902261967));
#16353=CARTESIAN_POINT('Ctrl Pts',(-15.8906015391955,-10.3204292252429,
-19.7454246750972));
#16354=CARTESIAN_POINT('Ctrl Pts',(-16.200456592374,-10.2641568661887,-19.5007816886992));
#16355=CARTESIAN_POINT('Ctrl Pts',(-16.6444363232276,-10.1320758235242,
-19.1203465671852));
#16356=CARTESIAN_POINT('Ctrl Pts',(-16.7876108033257,-10.0797343600817,
-18.9927696062974));
#16357=CARTESIAN_POINT('Ctrl Pts',(-16.987782528413,-9.97756209826158,-18.7983401508663));
#16358=CARTESIAN_POINT('Ctrl Pts',(-17.0519099637413,-9.93927191795146,
-18.732995983382));
#16359=CARTESIAN_POINT('Ctrl Pts',(-17.1734828765201,-9.85746485958505,
-18.5981367262514));
#16360=CARTESIAN_POINT('Ctrl Pts',(-17.2308500451718,-9.81433249494389,
-18.5283528074946));
#16361=CARTESIAN_POINT('Ctrl Pts',(-17.2858341932293,-9.77439024390244,
-18.4545876051761));
#16362=CARTESIAN_POINT('Ctrl Pts',(1.18948320324198E-15,10.75,-25.));
#16363=CARTESIAN_POINT('Ctrl Pts',(1.18948320324198E-15,10.75,-25.));
#16364=CARTESIAN_POINT('Ctrl Pts',(1.18948320324198E-15,10.75,-25.));
#16365=CARTESIAN_POINT('Ctrl Pts',(0.245046068213596,10.75,-26.0262609450161));
#16366=CARTESIAN_POINT('Ctrl Pts',(0.697525526338158,10.7499999999999,-25.5161823337686));
#16367=CARTESIAN_POINT('Ctrl Pts',(1.15008999572769,10.7499999999998,-25.0067283146802));
#16368=CARTESIAN_POINT('Ctrl Pts',(0.496527090381721,10.7416099797658,-27.00122252098));
#16369=CARTESIAN_POINT('Ctrl Pts',(1.34414287478967,10.7106845238825,-25.9683849162194));
#16370=CARTESIAN_POINT('Ctrl Pts',(2.19070342072973,10.749484751575,-24.9351054845997));
#16371=CARTESIAN_POINT('Ctrl Pts',(1.00994300948597,10.7055471241071,-28.8607675866388));
#16372=CARTESIAN_POINT('Ctrl Pts',(2.54379890611781,10.5691512799226,-26.7760314748787));
#16373=CARTESIAN_POINT('Ctrl Pts',(4.09237376657161,10.7476337609872,-24.7054729284982));
#16374=CARTESIAN_POINT('Ctrl Pts',(1.27181081709597,10.6778869683601,-29.7457578698098));
#16375=CARTESIAN_POINT('Ctrl Pts',(3.0977626829763,10.4667614319515,-27.1321627163013));
#16376=CARTESIAN_POINT('Ctrl Pts',(4.95399181959426,10.7462982551885,-24.5469284871057));
#16377=CARTESIAN_POINT('Ctrl Pts',(1.80395268087472,10.6009682382658,-31.4369952413203));
#16378=CARTESIAN_POINT('Ctrl Pts',(4.12187807240196,10.2129703311935,-27.7695605671644));
#16379=CARTESIAN_POINT('Ctrl Pts',(6.53563598753902,10.7430008170775,-24.1828886315384));
#16380=CARTESIAN_POINT('Ctrl Pts',(2.07423302929861,10.5517189359568,-32.2432082848239));
#16381=CARTESIAN_POINT('Ctrl Pts',(4.59231660943448,10.0612947296318,-28.0508074627162));
#16382=CARTESIAN_POINT('Ctrl Pts',(7.25565349942215,10.7410386985122,-23.9770771406387));
#16383=CARTESIAN_POINT('Ctrl Pts',(2.48491499500549,10.459798098358,-33.3988108702572));
#16384=CARTESIAN_POINT('Ctrl Pts',(5.23932024907478,9.80660117582193,-28.4255319484534));
#16385=CARTESIAN_POINT('Ctrl Pts',(8.2516652081245,10.7377584482577,-23.6501713365951));
#16386=CARTESIAN_POINT('Ctrl Pts',(2.62268926997547,10.4261480597688,-33.7750338413453));
#16387=CARTESIAN_POINT('Ctrl Pts',(5.445507716182,9.7170003420557,-28.5427016972242));
#16388=CARTESIAN_POINT('Ctrl Pts',(8.56961785745803,10.736608712042,-23.5380644347089));
#16389=CARTESIAN_POINT('Ctrl Pts',(2.89985851712585,10.3524819706058,-34.5101434304064));
#16390=CARTESIAN_POINT('Ctrl Pts',(5.83911442522935,9.53010244159021,-28.7624286517655));
#16391=CARTESIAN_POINT('Ctrl Pts',(9.18050627991221,10.7342176814138,-23.309481965988));
#16392=CARTESIAN_POINT('Ctrl Pts',(3.03960350978844,10.3123489874894,-34.8698754329864));
#16393=CARTESIAN_POINT('Ctrl Pts',(6.02694125231312,9.43251761880773,-28.8651891737879));
#16394=CARTESIAN_POINT('Ctrl Pts',(9.47410804615325,10.7329731060527,-23.1927050718314));
#16395=CARTESIAN_POINT('Ctrl Pts',(3.73556853847811,10.0969166520386,-36.6103249476162));
#16396=CARTESIAN_POINT('Ctrl Pts',(6.91528845301335,8.93215374352083,-29.3418543865727));
#16397=CARTESIAN_POINT('Ctrl Pts',(10.8737520565665,10.7266325629012,-22.6069251683481));
#16398=CARTESIAN_POINT('Ctrl Pts',(4.28614638192447,9.87708772192159,-37.826697916169));
#16399=CARTESIAN_POINT('Ctrl Pts',(7.45637148948174,8.49742418453718,-29.602022740049));
#16400=CARTESIAN_POINT('Ctrl Pts',(11.7860488717805,10.7211810673495,-22.1329942376077));
#16401=CARTESIAN_POINT('Ctrl Pts',(5.0963672454787,9.4699996867828,-39.4245954567253));
#16402=CARTESIAN_POINT('Ctrl Pts',(8.07481027224274,7.86615486907342,-29.8600948205774));
#16403=CARTESIAN_POINT('Ctrl Pts',(12.9720188548844,10.7133699557624,-21.4455568975883));
#16404=CARTESIAN_POINT('Ctrl Pts',(5.36385054816428,9.32136836042203,-39.9190359944775));
#16405=CARTESIAN_POINT('Ctrl Pts',(8.24891439461379,7.65822546479542,-29.9237161259567));
#16406=CARTESIAN_POINT('Ctrl Pts',(13.3360751704533,10.7108238630695,-21.2197719172396));
#16407=CARTESIAN_POINT('Ctrl Pts',(5.76043976597216,9.07765988049985,-40.6045618673102));
#16408=CARTESIAN_POINT('Ctrl Pts',(8.46797828230607,7.35877187776432,-29.9886773212175));
#16409=CARTESIAN_POINT('Ctrl Pts',(13.8455182988732,10.7071845019373,-20.8868823761153));
#16410=CARTESIAN_POINT('Ctrl Pts',(5.89186327262075,8.99295832117378,-40.8236913089109));
#16411=CARTESIAN_POINT('Ctrl Pts',(8.53406163401868,7.26085797953908,-30.0052396236136));
#16412=CARTESIAN_POINT('Ctrl Pts',(14.0091990780795,10.7060011866232,-20.776867418932));
#16413=CARTESIAN_POINT('Ctrl Pts',(6.15303145469192,8.81632327601466,-41.2430881438596));
#16414=CARTESIAN_POINT('Ctrl Pts',(8.65338623470555,7.0702484949104,-30.0285576176001));
#16415=CARTESIAN_POINT('Ctrl Pts',(14.3256984048538,10.7037082551722,-20.558718370803));
#16416=CARTESIAN_POINT('Ctrl Pts',(6.28222851753279,8.72473808032663,-41.4424366493991));
#16417=CARTESIAN_POINT('Ctrl Pts',(8.70631822359822,6.97798667254651,-30.0352185638796));
#16418=CARTESIAN_POINT('Ctrl Pts',(14.477836323313,10.7026036472603,-20.4510417895244));
#16419=CARTESIAN_POINT('Ctrl Pts',(6.91629337004597,8.25388281285371,-42.3814019788258));
#16420=CARTESIAN_POINT('Ctrl Pts',(8.9406909271843,6.53586785451668,-30.0452464088025));
#16421=CARTESIAN_POINT('Ctrl Pts',(15.2065644764352,10.6973537864051,-19.9232208998721));
#16422=CARTESIAN_POINT('Ctrl Pts',(7.39039954503924,7.83295516260841,-42.9577462278353));
#16423=CARTESIAN_POINT('Ctrl Pts',(9.02974447053307,6.24844545280141,-29.9797120750833));
#16424=CARTESIAN_POINT('Ctrl Pts',(15.6948891209362,10.6940034271962,-19.531025658328));
#16425=CARTESIAN_POINT('Ctrl Pts',(8.04909500484054,7.13282851376216,-43.5698483134004));
#16426=CARTESIAN_POINT('Ctrl Pts',(9.10228415305519,5.93399688656796,-29.7960167983354));
#16427=CARTESIAN_POINT('Ctrl Pts',(16.3457316620975,10.6904299449694,-18.974403503624));
#16428=CARTESIAN_POINT('Ctrl Pts',(8.25987706424816,6.88793250317514,-43.7313745857451));
#16429=CARTESIAN_POINT('Ctrl Pts',(9.11608373612093,5.84839107297692,-29.720008510016));
#16430=CARTESIAN_POINT('Ctrl Pts',(16.5486921403279,10.689477554208,-18.7941096079141));
#16431=CARTESIAN_POINT('Ctrl Pts',(8.56208087001458,6.50230282257969,-43.9067575462143));
#16432=CARTESIAN_POINT('Ctrl Pts',(9.13151165563714,5.74910282760032,-29.5847428654585));
#16433=CARTESIAN_POINT('Ctrl Pts',(16.8372849537151,10.6884006065242,-18.529572915309));
#16434=CARTESIAN_POINT('Ctrl Pts',(8.66022380779703,6.37099391565267,-43.9538118068111));
#16435=CARTESIAN_POINT('Ctrl Pts',(9.13576418549185,5.72095061553692,-29.5361224596565));
#16436=CARTESIAN_POINT('Ctrl Pts',(16.9305840559707,10.6881012822043,-18.4425923687403));
#16437=CARTESIAN_POINT('Ctrl Pts',(8.8493007701133,6.10564621923756,-44.0242038964039));
#16438=CARTESIAN_POINT('Ctrl Pts',(9.1441453636259,5.67452070070428,-29.433096998466));
#16439=CARTESIAN_POINT('Ctrl Pts',(17.1103836553971,10.6876194863027,-18.2724145506196));
#16440=CARTESIAN_POINT('Ctrl Pts',(8.94054219798202,5.97122136470861,-44.0477302440229));
#16441=CARTESIAN_POINT('Ctrl Pts',(9.14828867279214,5.65615432282493,-29.3785610731016));
#16442=CARTESIAN_POINT('Ctrl Pts',(17.1971766388057,10.6874358663274,-18.1889498564782));
#16443=CARTESIAN_POINT('Ctrl Pts',(9.38050433358115,5.2904733750073,-44.107352693009));
#16444=CARTESIAN_POINT('Ctrl Pts',(9.17283018200081,5.58622893796518,-29.090533858496));
#16445=CARTESIAN_POINT('Ctrl Pts',(17.6179260955997,10.6867755888011,-17.7785353846934));
#16446=CARTESIAN_POINT('Ctrl Pts',(9.68088377276865,4.71847711576924,-43.9723394445427));
#16447=CARTESIAN_POINT('Ctrl Pts',(9.20581394705623,5.6020000751546,-28.8151049209875));
#16448=CARTESIAN_POINT('Ctrl Pts',(17.9128300661226,10.6870812468964,-17.4724781037204));
#16449=CARTESIAN_POINT('Ctrl Pts',(9.99167371036606,3.96929102897458,-43.5523436135202));
#16450=CARTESIAN_POINT('Ctrl Pts',(9.31436628094941,5.66746485109492,-28.3999214292906));
#16451=CARTESIAN_POINT('Ctrl Pts',(18.2576364885818,10.6879612000447,-17.0983927259223));
#16452=CARTESIAN_POINT('Ctrl Pts',(10.0507078465258,3.8173439659351,-43.4552961639203));
#16453=CARTESIAN_POINT('Ctrl Pts',(9.33945467363902,5.68285111414041,-28.3129657645239));
#16454=CARTESIAN_POINT('Ctrl Pts',(18.3255411720261,10.6881621027409,-17.0238005943171));
#16455=CARTESIAN_POINT('Ctrl Pts',(10.1613705280416,3.51217769515195,-43.2359489845758));
#16456=CARTESIAN_POINT('Ctrl Pts',(9.39675929204993,5.71656007066854,-28.1321634865455));
#16457=CARTESIAN_POINT('Ctrl Pts',(18.4585717259105,10.688593493992,-16.8759350582039));
#16458=CARTESIAN_POINT('Ctrl Pts',(10.2130004334529,3.35902467638717,-43.1137730065085));
#16459=CARTESIAN_POINT('Ctrl Pts',(9.42893767601802,5.73485848796525,-28.0383919291859));
#16460=CARTESIAN_POINT('Ctrl Pts',(18.523680749316,10.688823741373,-16.802686410844));
#16461=CARTESIAN_POINT('Ctrl Pts',(10.3585730208717,2.89301393022493,-42.7045468149934));
#16462=CARTESIAN_POINT('Ctrl Pts',(9.53795019582644,5.79253740801612,-27.742635355066));
#16463=CARTESIAN_POINT('Ctrl Pts',(18.7178877558875,10.6895397789956,-16.5816878060987));
#16464=CARTESIAN_POINT('Ctrl Pts',(10.4412106167598,2.57843802764464,-42.3776190376175));
#16465=CARTESIAN_POINT('Ctrl Pts',(9.62664120261532,5.83414790030021,-27.5290499620756));
#16466=CARTESIAN_POINT('Ctrl Pts',(18.8436728070495,10.6900438144683,-16.4351079512893));
#16467=CARTESIAN_POINT('Ctrl Pts',(10.5093104711087,2.26205520585223,-41.9936955868538));
#16468=CARTESIAN_POINT('Ctrl Pts',(9.73208854678316,5.87295961250848,-27.2952574730422));
#16469=CARTESIAN_POINT('Ctrl Pts',(18.9678208753932,10.6905025318783,-16.2871078512552));
#16470=CARTESIAN_POINT('',(17.2858341932211,9.77439024389776,-18.4545876051875));
#16471=CARTESIAN_POINT('Ctrl Pts',(4.08240831242321E-16,10.75,-25.));
#16472=CARTESIAN_POINT('Ctrl Pts',(1.58979632319949,10.75,-25.016172365722));
#16473=CARTESIAN_POINT('Ctrl Pts',(3.17967643758184,10.7483783455921,-24.8861937318559));
#16474=CARTESIAN_POINT('Ctrl Pts',(6.30793928507803,10.7354991807564,-24.3342319030064));
#16475=CARTESIAN_POINT('Ctrl Pts',(7.84472428332795,10.7247729855381,-23.9141859389731));
#16476=CARTESIAN_POINT('Ctrl Pts',(10.0760168613779,10.6880402750733,-23.079902493822));
#16477=CARTESIAN_POINT('Ctrl Pts',(10.8051602307991,10.6723084956849,-22.768776762155));
#16478=CARTESIAN_POINT('Ctrl Pts',(12.2341014639881,10.6275778161733,-22.0805919845467));
#16479=CARTESIAN_POINT('Ctrl Pts',(12.9348666409494,10.598825513122,-21.7028235613454));
#16480=CARTESIAN_POINT('Ctrl Pts',(14.2895326619036,10.5142209407937,-20.8884435700631));
#16481=CARTESIAN_POINT('Ctrl Pts',(14.94591224686,10.4612196290951,-20.4513902262047));
#16482=CARTESIAN_POINT('Ctrl Pts',(15.8906015391836,10.3204292252449,-19.7454246751064));
#16483=CARTESIAN_POINT('Ctrl Pts',(16.200456592362,10.2641568661912,-19.5007816887089));
#16484=CARTESIAN_POINT('Ctrl Pts',(16.6444363232158,10.1320758235282,-19.1203465671956));
#16485=CARTESIAN_POINT('Ctrl Pts',(16.7876108033141,10.0797343600865,-18.9927696063079));
#16486=CARTESIAN_POINT('Ctrl Pts',(16.9877825284021,9.9775620982677,-18.7983401508771));
#16487=CARTESIAN_POINT('Ctrl Pts',(17.0519099637308,9.93927191795807,-18.732995983393));
#16488=CARTESIAN_POINT('Ctrl Pts',(17.1734828765102,9.85746485959219,-18.598136726263));
#16489=CARTESIAN_POINT('Ctrl Pts',(17.2308500451622,9.81433249495098,-18.5283528075066));
#16490=CARTESIAN_POINT('Ctrl Pts',(17.2858341932211,9.77439024389776,-18.4545876051875));
#16491=CARTESIAN_POINT('Origin',(49.598387070549,10.75,-42.0119030752));
#16492=CARTESIAN_POINT('Ctrl Pts',(10.5060622858798,2.27709359605911,-42.0119030752));
#16493=CARTESIAN_POINT('Ctrl Pts',(9.72158531033336,5.89651617104406,-27.202410868965));
#16494=CARTESIAN_POINT('Ctrl Pts',(19.0763027194419,10.75,-16.1584242596923));
#16495=CARTESIAN_POINT('Ctrl Pts',(10.5861279548434,1.90768633649479,-41.5656624370432));
#16496=CARTESIAN_POINT('Ctrl Pts',(10.054211023759,4.97457944703935,-27.0105294870069));
#16497=CARTESIAN_POINT('Ctrl Pts',(19.2216718028963,9.00616861666905,-15.9868045152509));
#16498=CARTESIAN_POINT('Ctrl Pts',(10.6468390893591,1.5338046393487,-41.2156085744635));
#16499=CARTESIAN_POINT('Ctrl Pts',(10.311656332032,4.01333959595599,-26.8528714213348));
#16500=CARTESIAN_POINT('Ctrl Pts',(19.3319171300874,7.2409846927467,-15.8521571440408));
#16501=CARTESIAN_POINT('Ctrl Pts',(10.728725307307,0.776010661488396,-40.7396085635752));
#16502=CARTESIAN_POINT('Ctrl Pts',(10.6587854631906,2.04350040512914,-26.6371988427527));
#16503=CARTESIAN_POINT('Ctrl Pts',(19.4806014076874,3.66349219260051,-15.6690802167434));
#16504=CARTESIAN_POINT('Ctrl Pts',(10.7498997026982,0.392119563052058,-40.6138592138001));
#16505=CARTESIAN_POINT('Ctrl Pts',(10.7495724464119,1.03183653258076,-26.578717448758));
#16506=CARTESIAN_POINT('Ctrl Pts',(19.5190486552012,1.85116909998997,-15.6207150822312));
#16507=CARTESIAN_POINT('Ctrl Pts',(10.7500246316439,-0.094580678063645,
-40.6131222287913));
#16508=CARTESIAN_POINT('Ctrl Pts',(10.7501050007708,-0.248881490684259,
-26.5783781675765));
#16509=CARTESIAN_POINT('Ctrl Pts',(19.5192754939424,-0.446508782486515,
-15.6204316264581));
#16510=CARTESIAN_POINT('Ctrl Pts',(10.7487192580301,-0.19226312690224,-40.6208265772758));
#16511=CARTESIAN_POINT('Ctrl Pts',(10.744538224302,-0.505954113601848,-26.5819274926781));
#16512=CARTESIAN_POINT('Ctrl Pts',(19.5169052717251,-0.90766080839821,-15.6233948374125));
#16513=CARTESIAN_POINT('Ctrl Pts',(10.7434916310807,-0.386417353144142,
-40.6516369832357));
#16514=CARTESIAN_POINT('Ctrl Pts',(10.722261359959,-1.01646923646688,-26.5960974937392));
#16515=CARTESIAN_POINT('Ctrl Pts',(19.5074132478589,-1.82424936484402,-15.6352449935534));
#16516=CARTESIAN_POINT('Ctrl Pts',(10.7395716055577,-0.483128018904152,
-40.6747296691341));
#16517=CARTESIAN_POINT('Ctrl Pts',(10.7055561163698,-1.27059431610844,-26.6067148813108));
#16518=CARTESIAN_POINT('Ctrl Pts',(19.500295491297,-2.280813670639,-15.6441267958185));
#16519=CARTESIAN_POINT('Ctrl Pts',(10.7239671336519,-0.772186979014415,
-40.7664424451147));
#16520=CARTESIAN_POINT('Ctrl Pts',(10.6391149691279,-2.02907825197572,-26.6487780897117));
#16521=CARTESIAN_POINT('Ctrl Pts',(19.4719617901052,-3.64544085441996,-15.6794009404334));
#16522=CARTESIAN_POINT('Ctrl Pts',(10.708441911361,-0.963462269665522,-40.8575101572767));
#16523=CARTESIAN_POINT('Ctrl Pts',(10.5730189889097,-2.52952302522834,-26.690482244076));
#16524=CARTESIAN_POINT('Ctrl Pts',(19.4437719857254,-4.54843815679182,-15.7144269835597));
#16525=CARTESIAN_POINT('Ctrl Pts',(10.6469585658024,-1.53320714658275,-41.2149233163682));
#16526=CARTESIAN_POINT('Ctrl Pts',(10.3121595644647,-4.01182480387279,-26.8525659713593));
#16527=CARTESIAN_POINT('Ctrl Pts',(19.3321340685354,-7.23816397107918,-15.851893583235));
#16528=CARTESIAN_POINT('Ctrl Pts',(10.5861513134375,-1.90757856453282,-41.5655322494299));
#16529=CARTESIAN_POINT('Ctrl Pts',(10.0543097325423,-4.97430585629965,-27.0104725449811));
#16530=CARTESIAN_POINT('Ctrl Pts',(19.2217159888502,-9.00563856695809,-15.9867523502243));
#16531=CARTESIAN_POINT('Ctrl Pts',(10.50606228588,-2.27709359605839,-42.0119030751991));
#16532=CARTESIAN_POINT('Ctrl Pts',(9.72158531033401,-5.89651617104224,-27.2024108689646));
#16533=CARTESIAN_POINT('Ctrl Pts',(19.0763027194422,-10.7499999999966,-16.158424259692));
#16534=CARTESIAN_POINT('Origin',(58.1890815764933,11.0623060762929,-60.5701598045158));
#16535=CARTESIAN_POINT('',(17.2858341932297,-9.77439024390216,-18.4545876051755));
#16536=CARTESIAN_POINT('Origin',(58.687261606127,-11.0785103164459,-61.1099573921991));
#16537=CARTESIAN_POINT('Origin',(49.5983870705491,-10.7499999999994,-42.0119030751999));
#16538=CARTESIAN_POINT('Ctrl Pts',(2.5146574731546E-15,-10.75,-25.));
#16539=CARTESIAN_POINT('Ctrl Pts',(2.5146574731546E-15,-10.75,-25.));
#16540=CARTESIAN_POINT('Ctrl Pts',(2.5146574731546E-15,-10.75,-25.));
#16541=CARTESIAN_POINT('Ctrl Pts',(1.15016130072756,-10.7499999999999,-25.0066480462939));
#16542=CARTESIAN_POINT('Ctrl Pts',(0.697561172183379,-10.75,-25.5161421503232));
#16543=CARTESIAN_POINT('Ctrl Pts',(0.245046068221819,-10.75,-26.0262609450183));
#16544=CARTESIAN_POINT('Ctrl Pts',(2.1908367452987,-10.7494908626442,-24.9349427537218));
#16545=CARTESIAN_POINT('Ctrl Pts',(1.34420967820515,-10.7106820865303,-25.9683035148595));
#16546=CARTESIAN_POINT('Ctrl Pts',(0.496527090381256,-10.7416099797658,
-27.001222520974));
#16547=CARTESIAN_POINT('Ctrl Pts',(4.09261727898974,-10.7476618291889,-24.7051473346811));
#16548=CARTESIAN_POINT('Ctrl Pts',(2.5439199817105,-10.5691405134721,-26.7758669153147));
#16549=CARTESIAN_POINT('Ctrl Pts',(1.00994300948646,-10.7055471241071,-28.8607675866448));
#16550=CARTESIAN_POINT('Ctrl Pts',(4.95428339066113,-10.746342167033,-24.5465224064888));
#16551=CARTESIAN_POINT('Ctrl Pts',(3.09790697546993,-10.4667447480452,-27.1319561817229));
#16552=CARTESIAN_POINT('Ctrl Pts',(1.27181081709445,-10.6778869683603,-29.7457578698038));
#16553=CARTESIAN_POINT('Ctrl Pts',(6.53601411261396,-10.7430838540963,-24.182326766051));
#16554=CARTESIAN_POINT('Ctrl Pts',(4.12206174340227,-10.2129395865731,-27.7692699618903));
#16555=CARTESIAN_POINT('Ctrl Pts',(1.8039526808771,-10.6009682382655,-31.4369952413291));
#16556=CARTESIAN_POINT('Ctrl Pts',(7.25607005425798,-10.7411450197821,-23.976439997658));
#16557=CARTESIAN_POINT('Ctrl Pts',(4.59251646503464,-10.0612558055132,-28.0504747196604));
#16558=CARTESIAN_POINT('Ctrl Pts',(2.07423302930479,-10.5517189359555,-32.2432082848164));
#16559=CARTESIAN_POINT('Ctrl Pts',(8.25213508492983,-10.7379037029823,-23.6494264617979));
#16560=CARTESIAN_POINT('Ctrl Pts',(5.23953945715423,-9.80654919147577,-28.4251361523469));
#16561=CARTESIAN_POINT('Ctrl Pts',(2.48491499500436,-10.4597980983582,-33.3988108702665));
#16562=CARTESIAN_POINT('Ctrl Pts',(8.57010470803834,-10.7367676144205,-23.5372845336702));
#16563=CARTESIAN_POINT('Ctrl Pts',(5.44573258389908,-9.71694385081973,-28.5422848859336));
#16564=CARTESIAN_POINT('Ctrl Pts',(2.6226892699774,-10.4261480597683,-33.7750338413409));
#16565=CARTESIAN_POINT('Ctrl Pts',(9.18102596589203,-10.7344049688864,-23.3086338762266));
#16566=CARTESIAN_POINT('Ctrl Pts',(5.83934903650617,-9.53003679931801,-28.7619698694455));
#16567=CARTESIAN_POINT('Ctrl Pts',(2.89985851712777,-10.3524819706052,-34.5101434304211));
#16568=CARTESIAN_POINT('Ctrl Pts',(9.47464363167845,-10.7331751699807,-23.19182374603));
#16569=CARTESIAN_POINT('Ctrl Pts',(6.02717995036764,-9.43244731739938,-28.8647093797186));
#16570=CARTESIAN_POINT('Ctrl Pts',(3.03960350978804,-10.3123489874896,-34.8698754329789));
#16571=CARTESIAN_POINT('Ctrl Pts',(10.8743638418358,-10.7269099179295,-22.6058842885203));
#16572=CARTESIAN_POINT('Ctrl Pts',(6.9155438867963,-8.93206017561179,-29.3412704946376));
#16573=CARTESIAN_POINT('Ctrl Pts',(3.73556853848941,-10.096916652035,-36.6103249476706));
#16574=CARTESIAN_POINT('Ctrl Pts',(11.7867149373558,-10.7215231826189,-22.1318452400645));
#16575=CARTESIAN_POINT('Ctrl Pts',(7.45662735841948,-8.49731283179493,-29.60135892625));
#16576=CARTESIAN_POINT('Ctrl Pts',(4.28614638190404,-9.87708772193193,-37.8266979161703));
#16577=CARTESIAN_POINT('Ctrl Pts',(12.9727669650347,-10.7138049243545,-21.444271498791));
#16578=CARTESIAN_POINT('Ctrl Pts',(8.07505237652506,-7.86602449975255,-29.85931736525));
#16579=CARTESIAN_POINT('Ctrl Pts',(5.0963672454905,-9.46999968677684,-39.4245954567278));
#16580=CARTESIAN_POINT('Ctrl Pts',(13.3368504702101,-10.7112891100125,-21.2184454394017));
#16581=CARTESIAN_POINT('Ctrl Pts',(8.24914946888037,-7.65808995232061,-29.9229017098166));
#16582=CARTESIAN_POINT('Ctrl Pts',(5.36385054816107,-9.32136836042409,-39.9190359944892));
#16583=CARTESIAN_POINT('Ctrl Pts',(13.8463349889244,-10.7076930483989,-20.8855001188216));
#16584=CARTESIAN_POINT('Ctrl Pts',(8.46819967604661,-7.35863132536776,-29.9878092669635));
#16585=CARTESIAN_POINT('Ctrl Pts',(5.76043976597773,-9.07765988049636,-40.6045618673112));
#16586=CARTESIAN_POINT('Ctrl Pts',(14.0100296238394,-10.7065238154119,-20.775467569332));
#16587=CARTESIAN_POINT('Ctrl Pts',(8.53427793972743,-7.26071617975511,-30.0043539623503));
#16588=CARTESIAN_POINT('Ctrl Pts',(5.89186327262587,-8.99295832117042,-40.8236913089118));
#16589=CARTESIAN_POINT('Ctrl Pts',(14.3265568770982,-10.7042581794669,-20.5572852081084));
#16590=CARTESIAN_POINT('Ctrl Pts',(8.65359140760035,-7.07010521633929,-30.027637381082));
#16591=CARTESIAN_POINT('Ctrl Pts',(6.15303145469467,-8.81632327601274,-41.2430881438715));
#16592=CARTESIAN_POINT('Ctrl Pts',(14.4787088144407,-10.7031667250934,-20.4495929775344));
#16593=CARTESIAN_POINT('Ctrl Pts',(8.70651736835601,-6.97784317275147,-30.0342814337065));
#16594=CARTESIAN_POINT('Ctrl Pts',(6.28222851753718,-8.72473808032344,-41.4424366494097));
#16595=CARTESIAN_POINT('Ctrl Pts',(15.2075064279654,-10.6979794034415,-19.9216993076092));
#16596=CARTESIAN_POINT('Ctrl Pts',(8.94085817952484,-6.53572591496858,-30.044227216124));
#16597=CARTESIAN_POINT('Ctrl Pts',(6.91629337004194,-8.25388281285646,-42.3814019788038));
#16598=CARTESIAN_POINT('Ctrl Pts',(15.6958870160119,-10.6946690258152,-19.5294613619358));
#16599=CARTESIAN_POINT('Ctrl Pts',(9.02988047150279,-6.24831400094229,-29.9786354100043));
#16600=CARTESIAN_POINT('Ctrl Pts',(7.3903995450421,-7.83295516260545,-42.9577462278144));
#16601=CARTESIAN_POINT('Ctrl Pts',(16.3468104233022,-10.6911383287306,-18.9727919246318));
#16602=CARTESIAN_POINT('Ctrl Pts',(9.10237199538834,-5.93389689679846,-29.794867977731));
#16603=CARTESIAN_POINT('Ctrl Pts',(8.04909500484009,-7.1328285137626,-43.5698483134118));
#16604=CARTESIAN_POINT('Ctrl Pts',(16.5497972768245,-10.6901973735152,-18.7924851417449));
#16605=CARTESIAN_POINT('Ctrl Pts',(9.11615526654625,-5.84830422616559,-29.7188379529152));
#16606=CARTESIAN_POINT('Ctrl Pts',(8.25987706424758,-6.88793250317606,-43.7313745857247));
#16607=CARTESIAN_POINT('Ctrl Pts',(16.8384281956481,-10.6891334162825,-18.5279328349385));
#16608=CARTESIAN_POINT('Ctrl Pts',(9.13155933367056,-5.74903976268807,-29.5835436932285));
#16609=CARTESIAN_POINT('Ctrl Pts',(8.562080870018,-6.50230282257525,-43.9067575462262));
#16610=CARTESIAN_POINT('Ctrl Pts',(16.931739712492,-10.6888377156648,-18.4409477322578));
#16611=CARTESIAN_POINT('Ctrl Pts',(9.13580402995641,-5.72089614985896,-29.5349144336253));
#16612=CARTESIAN_POINT('Ctrl Pts',(8.66022380779769,-6.37099391565181,-43.9538118068063));
#16613=CARTESIAN_POINT('Ctrl Pts',(17.1115632196287,-10.6883617817664,-18.2707620717659));
#16614=CARTESIAN_POINT('Ctrl Pts',(9.14417009997117,-5.67448453090892,-29.4318728599763));
#16615=CARTESIAN_POINT('Ctrl Pts',(8.84930077011531,-6.10564621923469,-44.0242038964098));
#16616=CARTESIAN_POINT('Ctrl Pts',(17.1983677384727,-10.6881804139003,-18.1872940720597));
#16617=CARTESIAN_POINT('Ctrl Pts',(9.14830611234615,-5.65612787409654,-29.3773296500064));
#16618=CARTESIAN_POINT('Ctrl Pts',(8.94054219798304,-5.97122136470706,-44.0477302440178));
#16619=CARTESIAN_POINT('Ctrl Pts',(17.6191724499837,-10.6875283412504,-17.7768660186183));
#16620=CARTESIAN_POINT('Ctrl Pts',(9.17281270066304,-5.58625383373677,-29.0892697905663));
#16621=CARTESIAN_POINT('Ctrl Pts',(9.38050433357937,-5.29047337500995,-44.10735269303));
#16622=CARTESIAN_POINT('Ctrl Pts',(17.914113305695,-10.6878306786809,-17.4708065259734));
#16623=CARTESIAN_POINT('Ctrl Pts',(9.20577390128042,-5.60207455122545,-28.8138272502701));
#16624=CARTESIAN_POINT('Ctrl Pts',(9.68088377276778,-4.71847711577154,-43.9723394445637));
#16625=CARTESIAN_POINT('Ctrl Pts',(18.2589536128454,-10.6887005830597,-17.0967283874812));
#16626=CARTESIAN_POINT('Ctrl Pts',(9.31430914664379,-5.66760810066136,-28.3986432457214));
#16627=CARTESIAN_POINT('Ctrl Pts',(9.99167371036688,-3.96929102897253,-43.5523436135141));
#16628=CARTESIAN_POINT('Ctrl Pts',(18.3268644816129,-10.6888991810849,-17.0221382282332));
#16629=CARTESIAN_POINT('Ctrl Pts',(9.33939467029628,-5.68300849364225,-28.311688314363));
#16630=CARTESIAN_POINT('Ctrl Pts',(10.0507078465264,-3.81734396593362,-43.4552961639137));
#16631=CARTESIAN_POINT('Ctrl Pts',(18.4599060816778,-10.6893256117491,-16.8742776734556));
#16632=CARTESIAN_POINT('Ctrl Pts',(9.39669478209269,-5.71674605355984,-28.1308891859807));
#16633=CARTESIAN_POINT('Ctrl Pts',(10.1613705280424,-3.51217769514969,-43.2359489845797));
#16634=CARTESIAN_POINT('Ctrl Pts',(18.5250199698833,-10.6895532060488,-16.8010320285879));
#16635=CARTESIAN_POINT('Ctrl Pts',(9.42887152573738,-5.7350589337783,-28.0371200401392));
#16636=CARTESIAN_POINT('Ctrl Pts',(10.2130004334531,-3.35902467638656,-43.1137730065023));
#16637=CARTESIAN_POINT('Ctrl Pts',(18.7174482790971,-10.6902544577855,-16.582082530172));
#16638=CARTESIAN_POINT('Ctrl Pts',(9.53687565009856,-5.79224964827862,-27.7441007582841));
#16639=CARTESIAN_POINT('Ctrl Pts',(10.35723024876,-2.89731244716951,-42.7083215470959));
#16640=CARTESIAN_POINT('Ctrl Pts',(18.8415673889002,-10.6907454914663,-16.437508385761));
#16641=CARTESIAN_POINT('Ctrl Pts',(9.62413494120418,-5.83327717253747,-27.5336719255695));
#16642=CARTESIAN_POINT('Ctrl Pts',(10.4389331022241,-2.58709663537585,-42.3866080951755));
#16643=CARTESIAN_POINT('Ctrl Pts',(18.9640552529202,-10.6911938869776,-16.2915947644372));
#16644=CARTESIAN_POINT('Ctrl Pts',(9.72768083152049,-5.87165945892117,-27.3036548029488));
#16645=CARTESIAN_POINT('Ctrl Pts',(10.5064904280776,-2.27511733550195,-42.0095150580982));
#16646=CARTESIAN_POINT('Ctrl Pts',(17.2858341932297,-9.77439024390216,-18.4545876051755));
#16647=CARTESIAN_POINT('Ctrl Pts',(17.2308496142754,-9.81433280796087,-18.5283533855733));
#16648=CARTESIAN_POINT('Ctrl Pts',(17.1734819746953,-9.85746553470452,-18.5981378177516));
#16649=CARTESIAN_POINT('Ctrl Pts',(17.0519080073576,-9.93927316613411,-18.7329980624534));
#16650=CARTESIAN_POINT('Ctrl Pts',(16.9877799937373,-9.97756355387054,-18.7983427112242));
#16651=CARTESIAN_POINT('Ctrl Pts',(16.7876064605028,-10.0797362530431,-18.9927736277445));
#16652=CARTESIAN_POINT('Ctrl Pts',(16.6444306883125,-10.1320778149369,-19.1203515704373));
#16653=CARTESIAN_POINT('Ctrl Pts',(16.2004469860554,-10.2641590938575,-19.5007895704323));
#16654=CARTESIAN_POINT('Ctrl Pts',(15.8905894180583,-10.3204314322062,-19.7454341656193));
#16655=CARTESIAN_POINT('Ctrl Pts',(14.9458920693915,-10.4612218351731,-20.451404439969));
#16656=CARTESIAN_POINT('Ctrl Pts',(14.289506801601,-10.5142230477086,-20.888460478508));
#16657=CARTESIAN_POINT('Ctrl Pts',(12.9348288042006,-10.5988273843318,-21.7028449453775));
#16658=CARTESIAN_POINT('Ctrl Pts',(12.2340573634716,-10.6275795411285,-22.0806151123363));
#16659=CARTESIAN_POINT('Ctrl Pts',(10.8051035470397,-10.672309925593,-22.7688021724104));
#16660=CARTESIAN_POINT('Ctrl Pts',(10.0759536654715,-10.6880415610146,-23.0799285438409));
#16661=CARTESIAN_POINT('Ctrl Pts',(7.8446408421546,-10.7247738680017,-23.9142122954435));
#16662=CARTESIAN_POINT('Ctrl Pts',(6.30784220188933,-10.7354998258494,-24.3342560266836));
#16663=CARTESIAN_POINT('Ctrl Pts',(3.9616252120437,-10.7451589131064,-24.7482204101398));
#16664=CARTESIAN_POINT('Ctrl Pts',(3.1741229733079,-10.7471212251943,-24.8500338800462));
#16665=CARTESIAN_POINT('Ctrl Pts',(1.98574081627453,-10.7489410804811,-24.9478353565517));
#16666=CARTESIAN_POINT('Ctrl Pts',(1.58913075295958,-10.749354887983,-24.971215877855));
#16667=CARTESIAN_POINT('Ctrl Pts',(0.794943421248738,-10.7498845226873,
-24.999500006716));
#16668=CARTESIAN_POINT('Ctrl Pts',(0.39613862981597,-10.75,-25.0040317726262));
#16669=CARTESIAN_POINT('Ctrl Pts',(0.,-10.75,-25.));
#16670=CARTESIAN_POINT('Origin',(0.,-5.75,0.));
#16671=CARTESIAN_POINT('',(-2.44929359829471E-15,-5.75,20.));
#16672=CARTESIAN_POINT('Origin',(0.,-5.75,0.));
#16673=CARTESIAN_POINT('',(-2.44929359829471E-15,-5.75,20.));
#16674=CARTESIAN_POINT('Origin',(0.,-5.75,0.));
#16675=CARTESIAN_POINT('Ctrl Pts',(16.4780203712966,-10.75,-17.8656547184251));
#16676=CARTESIAN_POINT('Ctrl Pts',(17.2666005308027,-10.75,-18.4405653935864));
#16677=CARTESIAN_POINT('Ctrl Pts',(17.2858341932296,-9.77439024390242,-18.4545876051757));
#16678=CARTESIAN_POINT('Ctrl Pts',(16.420186402265,-10.75,-17.9449830848012));
#16679=CARTESIAN_POINT('Ctrl Pts',(17.1646987553025,-10.75,-18.501481536098));
#16680=CARTESIAN_POINT('Ctrl Pts',(17.2188661426269,-9.82303803508069,-18.5444300755199));
#16681=CARTESIAN_POINT('Ctrl Pts',(16.3609340347876,-10.75,-18.0226389830102));
#16682=CARTESIAN_POINT('Ctrl Pts',(17.0565699547852,-10.75,-18.5602973050013));
#16683=CARTESIAN_POINT('Ctrl Pts',(17.1454229102231,-9.87836276842019,-18.6315395728602));
#16684=CARTESIAN_POINT('Ctrl Pts',(16.2394647608978,-10.75,-18.1745295246658));
#16685=CARTESIAN_POINT('Ctrl Pts',(16.8540047055405,-10.75,-18.6788326359785));
#16686=CARTESIAN_POINT('Ctrl Pts',(16.9922413943603,-9.97582686527392,-18.7950045725018));
#16687=CARTESIAN_POINT('Ctrl Pts',(16.1773081113179,-10.75,-18.2488221735799));
#16688=CARTESIAN_POINT('Ctrl Pts',(16.7583976671104,-10.75,-18.7391027373329));
#16689=CARTESIAN_POINT('Ctrl Pts',(16.9133187470164,-10.0176700000188,-18.8718344001156));
#16690=CARTESIAN_POINT('Ctrl Pts',(15.9875644144504,-10.75,-18.4678954650283));
#16691=CARTESIAN_POINT('Ctrl Pts',(16.4909861673415,-10.75,-18.9187569933654));
#16692=CARTESIAN_POINT('Ctrl Pts',(16.6765372063047,-10.1240114260747,-19.0935506433098));
#16693=CARTESIAN_POINT('Ctrl Pts',(15.8568225101407,-10.75,-18.6090096240716));
#16694=CARTESIAN_POINT('Ctrl Pts',(16.3229486004118,-10.75,-19.0436478681492));
#16695=CARTESIAN_POINT('Ctrl Pts',(16.5179814662752,-10.1729273502795,-19.2306007925836));
#16696=CARTESIAN_POINT('Ctrl Pts',(15.456057039199,-10.75,-19.022427441683));
#16697=CARTESIAN_POINT('Ctrl Pts',(15.8403045574758,-10.75,-19.4059080219916));
#16698=CARTESIAN_POINT('Ctrl Pts',(16.0415174065678,-10.2970310354253,-19.6286372648659));
#16699=CARTESIAN_POINT('Ctrl Pts',(15.1775121139788,-10.75,-19.2848278240102));
#16700=CARTESIAN_POINT('Ctrl Pts',(15.5212812150563,-10.75,-19.6505377189956));
#16701=CARTESIAN_POINT('Ctrl Pts',(15.7216572711278,-10.3488754024673,-19.8754301022883));
#16702=CARTESIAN_POINT('Ctrl Pts',(14.3174283733583,-10.75,-20.0436150917603));
#16703=CARTESIAN_POINT('Ctrl Pts',(14.580705202477,-10.75,-20.3431259159941));
#16704=CARTESIAN_POINT('Ctrl Pts',(14.7498205235968,-10.4800501520616,-20.5861008531719));
#16705=CARTESIAN_POINT('Ctrl Pts',(13.7112218641371,-10.75,-20.511333897607));
#16706=CARTESIAN_POINT('Ctrl Pts',(13.9284252758013,-10.75,-20.791177099007));
#16707=CARTESIAN_POINT('Ctrl Pts',(14.0859782414513,-10.5295463004069,-21.0183499982909));
#16708=CARTESIAN_POINT('Ctrl Pts',(12.4444282590119,-10.75,-21.3835719658819));
#16709=CARTESIAN_POINT('Ctrl Pts',(12.5993509724745,-10.75,-21.6142534710468));
#16710=CARTESIAN_POINT('Ctrl Pts',(12.7203223126435,-10.6086489117044,-21.8215270095858));
#16711=CARTESIAN_POINT('Ctrl Pts',(11.7822109370052,-10.75,-21.7877736287731));
#16712=CARTESIAN_POINT('Ctrl Pts',(11.9106547115043,-10.75,-21.9998133945429));
#16713=CARTESIAN_POINT('Ctrl Pts',(12.017568252458,-10.6355424608103,-22.1915948020144));
#16714=CARTESIAN_POINT('Ctrl Pts',(10.4276042052761,-10.75,-22.5220998589813));
#16715=CARTESIAN_POINT('Ctrl Pts',(10.5179685506165,-10.75,-22.6958229564124));
#16716=CARTESIAN_POINT('Ctrl Pts',(10.5948532243949,-10.6772804141921,-22.8609639240682));
#16717=CARTESIAN_POINT('Ctrl Pts',(9.73251018538536,-10.75,-22.8541153700672));
#16718=CARTESIAN_POINT('Ctrl Pts',(9.80642247244757,-10.75,-23.0117088133705));
#16719=CARTESIAN_POINT('Ctrl Pts',(9.87204995901033,-10.6919698658214,-23.1619487822205));
#16720=CARTESIAN_POINT('Ctrl Pts',(7.59539354894044,-10.75,-23.7477563831948));
#16721=CARTESIAN_POINT('Ctrl Pts',(7.63899237205308,-10.75,-23.8550327053113));
#16722=CARTESIAN_POINT('Ctrl Pts',(7.66543048577482,-10.7263148678223,-23.9669915332414));
#16723=CARTESIAN_POINT('Ctrl Pts',(6.11513874037308,-10.75,-24.2011081296479));
#16724=CARTESIAN_POINT('Ctrl Pts',(6.13861428587886,-10.7499999999906,-24.2845436650543));
#16725=CARTESIAN_POINT('Ctrl Pts',(6.15722358267718,-10.73636285653,-24.3678462428209));
#16726=CARTESIAN_POINT('Ctrl Pts',(3.08771028814334,-10.75,-24.8194092303925));
#16727=CARTESIAN_POINT('Ctrl Pts',(3.09355332608923,-10.7500000000094,-24.8560196583317));
#16728=CARTESIAN_POINT('Ctrl Pts',(3.09482729538435,-10.7484649507037,-24.8935813777596));
#16729=CARTESIAN_POINT('Ctrl Pts',(1.54655171301311,-10.75,-24.9814490353809));
#16730=CARTESIAN_POINT('Ctrl Pts',(1.54684319067375,-10.75,-24.9985607643983));
#16731=CARTESIAN_POINT('Ctrl Pts',(1.54703957001439,-10.75,-25.0156741335565));
#16732=CARTESIAN_POINT('Ctrl Pts',(0.,-10.75,-25.));
#16733=CARTESIAN_POINT('Ctrl Pts',(0.,-10.75,-25.));
#16734=CARTESIAN_POINT('Ctrl Pts',(0.,-10.75,-25.));
#16735=CARTESIAN_POINT('Origin',(16.4780203712966,-9.75,-17.8656547184251));
#16736=CARTESIAN_POINT('Ctrl Pts',(18.3893975112955,-10.75,-15.4217398231055));
#16737=CARTESIAN_POINT('Ctrl Pts',(19.1556224075994,-10.75,-16.064312315735));
#16738=CARTESIAN_POINT('Ctrl Pts',(19.1556224075994,-9.74999999999999,-16.064312315735));
#16739=CARTESIAN_POINT('Ctrl Pts',(17.7244639958846,-10.75,-16.214628749746));
#16740=CARTESIAN_POINT('Ctrl Pts',(18.5021835427803,-10.75,-16.8319676033546));
#16741=CARTESIAN_POINT('Ctrl Pts',(18.505450860098,-9.75743449038258,-16.8395985788077));
#16742=CARTESIAN_POINT('Ctrl Pts',(17.0876217955067,-10.75,-17.0294907556045));
#16743=CARTESIAN_POINT('Ctrl Pts',(17.8730318352358,-10.75,-17.623535138591));
#16744=CARTESIAN_POINT('Ctrl Pts',(17.8824917699952,-9.76550892523746,-17.6365459729584));
#16745=CARTESIAN_POINT('Ctrl Pts',(16.4780203712966,-10.75,-17.8656547184251));
#16746=CARTESIAN_POINT('Ctrl Pts',(17.2666005308027,-10.75,-18.4405653935864));
#16747=CARTESIAN_POINT('Ctrl Pts',(17.2858341932296,-9.77439024390236,-18.4545876051756));
#16748=CARTESIAN_POINT('Origin',(18.3893975112954,-9.75,-15.4217398231056));
#16749=CARTESIAN_POINT('Origin',(0.,-9.75,0.));
#16750=CARTESIAN_POINT('Origin',(-18.3893975112944,-9.75,-15.4217398231068));
#16751=CARTESIAN_POINT('Ctrl Pts',(-16.4780203712963,-10.75,-17.8656547184255));
#16752=CARTESIAN_POINT('Ctrl Pts',(-17.2666005308023,-10.75,-18.4405653935868));
#16753=CARTESIAN_POINT('Ctrl Pts',(-17.2858341932293,-9.77439024390244,
-18.4545876051761));
#16754=CARTESIAN_POINT('Ctrl Pts',(-17.0876217955269,-10.75,-17.0294907556188));
#16755=CARTESIAN_POINT('Ctrl Pts',(-17.8730318353556,-10.75,-17.6235351386676));
#16756=CARTESIAN_POINT('Ctrl Pts',(-17.8824917699965,-9.76550892511618,
-17.6365459729617));
#16757=CARTESIAN_POINT('Ctrl Pts',(-17.724463995877,-10.75,-16.2146287497442));
#16758=CARTESIAN_POINT('Ctrl Pts',(-18.5021835427599,-10.7499999999973,
-16.8319676033585));
#16759=CARTESIAN_POINT('Ctrl Pts',(-18.5054508600972,-9.75743449038529,
-16.8395985788087));
#16760=CARTESIAN_POINT('Ctrl Pts',(-18.3893975112945,-10.75,-15.4217398231068));
#16761=CARTESIAN_POINT('Ctrl Pts',(-19.1556224075984,-10.75,-16.0643123157362));
#16762=CARTESIAN_POINT('Ctrl Pts',(-19.1556224075984,-9.75,-16.0643123157362));
#16763=CARTESIAN_POINT('Origin',(-16.4780203712963,-9.75,-17.8656547184255));
#16764=CARTESIAN_POINT('Ctrl Pts',(-5.35841952801743E-40,-10.75,-25.));
#16765=CARTESIAN_POINT('Ctrl Pts',(-5.35841952801743E-40,-10.75,-25.));
#16766=CARTESIAN_POINT('Ctrl Pts',(-5.35841952801743E-40,-10.75,-25.));
#16767=CARTESIAN_POINT('Ctrl Pts',(-1.55042841078198,-10.75,-24.9814045184011));
#16768=CARTESIAN_POINT('Ctrl Pts',(-1.55072583154171,-10.75,-24.998585080049));
#16769=CARTESIAN_POINT('Ctrl Pts',(-1.55092559030133,-10.75,-25.0157668478768));
#16770=CARTESIAN_POINT('Ctrl Pts',(-3.07944423838035,-10.75,-24.8200362535366));
#16771=CARTESIAN_POINT('Ctrl Pts',(-3.08524485674213,-10.7499999999987,
-24.8565651264907));
#16772=CARTESIAN_POINT('Ctrl Pts',(-3.08654552726842,-10.7484627964799,
-24.8940268047827));
#16773=CARTESIAN_POINT('Ctrl Pts',(-5.33854036060754,-10.75,-24.3602374464479));
#16774=CARTESIAN_POINT('Ctrl Pts',(-5.3557332742001,-10.7500000000007,-24.4319952968947));
#16775=CARTESIAN_POINT('Ctrl Pts',(-5.37162508811807,-10.7394784010279,
-24.5032449016001));
#16776=CARTESIAN_POINT('Ctrl Pts',(-6.08590968694707,-10.75,-24.1707865634184));
#16777=CARTESIAN_POINT('Ctrl Pts',(-6.1094282435196,-10.7499999999987,-24.2548405732474));
#16778=CARTESIAN_POINT('Ctrl Pts',(-6.13034393953452,-10.7353379259098,
-24.3384029005633));
#16779=CARTESIAN_POINT('Ctrl Pts',(-7.56885814939832,-10.75,-23.7165457546288));
#16780=CARTESIAN_POINT('Ctrl Pts',(-7.60772303658771,-10.7500000000013,
-23.8278999852315));
#16781=CARTESIAN_POINT('Ctrl Pts',(-7.64328958394848,-10.7230487971063,
-23.9369917727021));
#16782=CARTESIAN_POINT('Ctrl Pts',(-8.29448746489639,-10.75,-23.4547722125325));
#16783=CARTESIAN_POINT('Ctrl Pts',(-8.343770430558,-10.7500000000007,-23.5802417303107));
#16784=CARTESIAN_POINT('Ctrl Pts',(-8.38736583248543,-10.7150024615342,
-23.7030917074376));
#16785=CARTESIAN_POINT('Ctrl Pts',(-9.71223839813022,-10.75,-22.8632329101288));
#16786=CARTESIAN_POINT('Ctrl Pts',(-9.78574594442074,-10.7499999999993,
-23.0204047949222));
#16787=CARTESIAN_POINT('Ctrl Pts',(-9.85107461164577,-10.692321177143,-23.1702735598621));
#16788=CARTESIAN_POINT('Ctrl Pts',(-10.4047291096027,-10.75,-22.5333929349819));
#16789=CARTESIAN_POINT('Ctrl Pts',(-10.4945435000878,-10.7499999999993,
-22.7066109051832));
#16790=CARTESIAN_POINT('Ctrl Pts',(-10.5710496564742,-10.677775627927,-22.8713056754172));
#16791=CARTESIAN_POINT('Ctrl Pts',(-11.7557843148556,-10.75,-21.8031670890272));
#16792=CARTESIAN_POINT('Ctrl Pts',(-11.8833543298829,-10.7500000000007,
-22.0144907873188));
#16793=CARTESIAN_POINT('Ctrl Pts',(-11.989696301555,-10.6364601057527,-22.2057694542664));
#16794=CARTESIAN_POINT('Ctrl Pts',(-12.41441707146,-10.75,-21.4029231633718));
#16795=CARTESIAN_POINT('Ctrl Pts',(-12.5682277181088,-10.7499999999993,
-21.6325922237354));
#16796=CARTESIAN_POINT('Ctrl Pts',(-12.6883191844485,-10.6100667089293,
-21.8393995383973));
#16797=CARTESIAN_POINT('Ctrl Pts',(-13.6941367871331,-10.75,-20.5243628920851));
#16798=CARTESIAN_POINT('Ctrl Pts',(-13.9104000254228,-10.7500000000007,
-20.8034739165238));
#16799=CARTESIAN_POINT('Ctrl Pts',(-14.0673658616455,-10.5308667062636,
-21.0305204614681));
#16800=CARTESIAN_POINT('Ctrl Pts',(-14.3061796724473,-10.75,-20.0529523054155));
#16801=CARTESIAN_POINT('Ctrl Pts',(-14.5687361887894,-10.75,-20.3518360674549));
#16802=CARTESIAN_POINT('Ctrl Pts',(-14.7373892678267,-10.4812146028895,
-20.5949120467487));
#16803=CARTESIAN_POINT('Ctrl Pts',(-15.1723199996605,-10.75,-19.2896963078701));
#16804=CARTESIAN_POINT('Ctrl Pts',(-15.5155349295134,-10.75,-19.6550871682641));
#16805=CARTESIAN_POINT('Ctrl Pts',(-15.7157951752577,-10.3496720503833,
-19.8801300237897));
#16806=CARTESIAN_POINT('Ctrl Pts',(-15.452535977331,-10.75,-19.0259122646854));
#16807=CARTESIAN_POINT('Ctrl Pts',(-15.8363472416202,-10.75,-19.4091372131905));
#16808=CARTESIAN_POINT('Ctrl Pts',(-16.0374978185796,-10.2976793876105,
-19.6320606736257));
#16809=CARTESIAN_POINT('Ctrl Pts',(-15.8551923244479,-10.75,-18.6107640482246));
#16810=CARTESIAN_POINT('Ctrl Pts',(-16.3210408269098,-10.75,-19.0453117612741));
#16811=CARTESIAN_POINT('Ctrl Pts',(-16.5161004001834,-10.1732729614044,
-19.2323970231278));
#16812=CARTESIAN_POINT('Ctrl Pts',(-15.9864615716645,-10.75,-18.4691305151303));
#16813=CARTESIAN_POINT('Ctrl Pts',(-16.4896849140115,-10.75,-18.9199442477269));
#16814=CARTESIAN_POINT('Ctrl Pts',(-16.6752619096529,-10.1242452909551,
-19.0948558730444));
#16815=CARTESIAN_POINT('Ctrl Pts',(-16.1767927349458,-10.75,-18.2494361858635));
#16816=CARTESIAN_POINT('Ctrl Pts',(-16.7578253325221,-10.75,-18.7397668697928));
#16817=CARTESIAN_POINT('Ctrl Pts',(-16.9127359309499,-10.0176850161698,
-18.8725266064876));
#16818=CARTESIAN_POINT('Ctrl Pts',(-16.2391104423901,-10.75,-18.174963720535));
#16819=CARTESIAN_POINT('Ctrl Pts',(-16.8536585339569,-10.75,-18.6793495841847));
#16820=CARTESIAN_POINT('Ctrl Pts',(-16.9918520227291,-9.97575786108518,
-18.7955142959009));
#16821=CARTESIAN_POINT('Ctrl Pts',(-16.4192374533764,-10.75,-17.9497511291255));
#16822=CARTESIAN_POINT('Ctrl Pts',(-17.160271716382,-10.75,-18.4999634281549));
#16823=CARTESIAN_POINT('Ctrl Pts',(-17.2189763207791,-9.83124367041143,
-18.5531344920881));
#16824=CARTESIAN_POINT('Ctrl Pts',(-16.5326524480039,-10.75,-17.7942078342577));
#16825=CARTESIAN_POINT('Ctrl Pts',(-17.390066786921,-10.75,-18.3836903792569));
#16826=CARTESIAN_POINT('Ctrl Pts',(-17.3570580545225,-9.71022120413227,
-18.3720918508499));
#16827=CARTESIAN_POINT('Ctrl Pts',(-16.640726582166,-10.75,-17.6325831459554));
#16828=CARTESIAN_POINT('Ctrl Pts',(-17.5392115108332,-10.75,-18.2500344325275));
#16829=CARTESIAN_POINT('Ctrl Pts',(-17.4577990624194,-9.66415958091025,
-18.190604719098));
#16830=CARTESIAN_POINT('Ctrl Pts',(6.03940677783316E-16,10.75,-25.));
#16831=CARTESIAN_POINT('Ctrl Pts',(6.03940677783316E-16,10.75,-25.));
#16832=CARTESIAN_POINT('Ctrl Pts',(6.03940677783316E-16,10.75,-25.));
#16833=CARTESIAN_POINT('Ctrl Pts',(0.77551876936987,10.75,-24.990698606333));
#16834=CARTESIAN_POINT('Ctrl Pts',(0.775625402192565,10.75,-24.9992899262904));
#16835=CARTESIAN_POINT('Ctrl Pts',(0.775729285272185,10.75,-25.0078813851305));
#16836=CARTESIAN_POINT('Ctrl Pts',(1.54921288772271,10.75,-24.9460692154471));
#16837=CARTESIAN_POINT('Ctrl Pts',(1.55044130692443,10.7500000000249,-24.9639270378186));
#16838=CARTESIAN_POINT('Ctrl Pts',(1.55122662830252,10.7495696386015,-24.9818302943601));
#16839=CARTESIAN_POINT('Ctrl Pts',(3.09087304220801,10.75,-24.7816780284712));
#16840=CARTESIAN_POINT('Ctrl Pts',(3.09605488960405,10.7499999999752,-24.8197202989179));
#16841=CARTESIAN_POINT('Ctrl Pts',(3.10078026619678,10.747267815588,-24.8577117264916));
#16842=CARTESIAN_POINT('Ctrl Pts',(3.85256422917062,10.75,-24.6633151125848));
#16843=CARTESIAN_POINT('Ctrl Pts',(3.86111871633922,10.7499999999973,-24.712078758921));
#16844=CARTESIAN_POINT('Ctrl Pts',(3.86850703318997,10.7454111698887,-24.7608678209163));
#16845=CARTESIAN_POINT('Ctrl Pts',(6.10952281364908,10.75,-24.2020255484112));
#16846=CARTESIAN_POINT('Ctrl Pts',(6.13294958208081,10.7500000000053,-24.2853845753718));
#16847=CARTESIAN_POINT('Ctrl Pts',(6.15155990520288,10.7363778606325,-24.3686028672562));
#16848=CARTESIAN_POINT('Ctrl Pts',(7.5775794845246,10.75,-23.7541652338085));
#16849=CARTESIAN_POINT('Ctrl Pts',(7.62096600221208,10.75,-23.8610830094627));
#16850=CARTESIAN_POINT('Ctrl Pts',(7.64716672681317,10.726508702728,-23.9727170011077));
#16851=CARTESIAN_POINT('Ctrl Pts',(9.72149591099175,10.75,-22.8592338757647));
#16852=CARTESIAN_POINT('Ctrl Pts',(9.79518731370962,10.75,-23.0165595755935));
#16853=CARTESIAN_POINT('Ctrl Pts',(9.86061355528561,10.6921924563451,-23.1665834858966));
#16854=CARTESIAN_POINT('Ctrl Pts',(10.4190640908032,10.75,-22.5262337182939));
#16855=CARTESIAN_POINT('Ctrl Pts',(10.5091983832299,10.7500000000007,-22.6997672275432));
#16856=CARTESIAN_POINT('Ctrl Pts',(10.585964436799,10.6774671158219,-22.8647134299696));
#16857=CARTESIAN_POINT('Ctrl Pts',(11.7684524650003,10.75,-21.7957196072559));
#16858=CARTESIAN_POINT('Ctrl Pts',(11.8964128840459,10.7499999999993,-22.0073671320669));
#16859=CARTESIAN_POINT('Ctrl Pts',(12.0030386260281,10.6360415664677,-22.1988562680654));
#16860=CARTESIAN_POINT('Ctrl Pts',(12.4221781820695,10.75,-21.3975520043717));
#16861=CARTESIAN_POINT('Ctrl Pts',(12.576137264646,10.75,-21.6275792716514));
#16862=CARTESIAN_POINT('Ctrl Pts',(12.6966279179313,10.6096487571098,-21.8343422634894));
#16863=CARTESIAN_POINT('Ctrl Pts',(13.684782342616,10.75,-20.530827861331));
#16864=CARTESIAN_POINT('Ctrl Pts',(13.9003194774231,10.75,-20.8096148861702));
#16865=CARTESIAN_POINT('Ctrl Pts',(14.0571943009162,10.5315720187492,-21.0363561860875));
#16866=CARTESIAN_POINT('Ctrl Pts',(14.294089112681,10.75,-20.0629435906517));
#16867=CARTESIAN_POINT('Ctrl Pts',(14.5557034416343,10.75,-20.3609974720801));
#16868=CARTESIAN_POINT('Ctrl Pts',(14.7238617885168,10.4827239049414,-20.6040773940109));
#16869=CARTESIAN_POINT('Ctrl Pts',(15.1661919626405,10.75,-19.2954210789481));
#16870=CARTESIAN_POINT('Ctrl Pts',(15.5085221078731,10.75,-19.6602020075858));
#16871=CARTESIAN_POINT('Ctrl Pts',(15.7086678083383,10.3510274540215,-19.8854122863091));
#16872=CARTESIAN_POINT('Ctrl Pts',(15.450317409084,10.75,-19.0281667232991));
#16873=CARTESIAN_POINT('Ctrl Pts',(15.8336640610588,10.75,-19.4109514699529));
#16874=CARTESIAN_POINT('Ctrl Pts',(16.0347782735401,10.2985349668086,-19.6341135503095));
#16875=CARTESIAN_POINT('Ctrl Pts',(15.8555452026401,10.75,-18.6104166452363));
#16876=CARTESIAN_POINT('Ctrl Pts',(16.3213284001396,10.75,-19.0448335078672));
#16877=CARTESIAN_POINT('Ctrl Pts',(16.5164212277897,10.1734575195196,-19.2319798190006));
#16878=CARTESIAN_POINT('Ctrl Pts',(15.987345897022,10.75,-18.4681633272427));
#16879=CARTESIAN_POINT('Ctrl Pts',(16.4906809550653,10.7500000000002,-18.9189415895965));
#16880=CARTESIAN_POINT('Ctrl Pts',(16.6762580682836,10.1241735884936,-19.0938318798831));
#16881=CARTESIAN_POINT('Ctrl Pts',(16.1778522854737,10.75,-18.2481860733963));
#16882=CARTESIAN_POINT('Ctrl Pts',(16.7592036816611,10.7499999999999,-18.7385719233192));
#16883=CARTESIAN_POINT('Ctrl Pts',(16.9140010589,10.0173451034587,-18.8711855370801));
#16884=CARTESIAN_POINT('Ctrl Pts',(16.2401220962037,10.75,-18.1737303235091));
#16885=CARTESIAN_POINT('Ctrl Pts',(16.8550468116417,10.75,-18.6781983255835));
#16886=CARTESIAN_POINT('Ctrl Pts',(16.9930765400665,9.97534637831806,-18.7941646549338));
#16887=CARTESIAN_POINT('Ctrl Pts',(16.3614947681369,10.75,-18.0219148278828));
#16888=CARTESIAN_POINT('Ctrl Pts',(17.0575602016681,10.75,-18.5597436355989));
#16889=CARTESIAN_POINT('Ctrl Pts',(17.1461237747635,9.87786543139612,-18.6307398467417));
#16890=CARTESIAN_POINT('Ctrl Pts',(16.4205359348328,10.75,-17.9445036454283));
#16891=CARTESIAN_POINT('Ctrl Pts',(17.1653078416885,10.75,-18.5011174272147));
#16892=CARTESIAN_POINT('Ctrl Pts',(17.219277234529,9.82273940521341,-18.5438785660551));
#16893=CARTESIAN_POINT('Ctrl Pts',(16.4780203712861,10.75,-17.8656547184465));
#16894=CARTESIAN_POINT('Ctrl Pts',(17.2666005307924,10.75,-18.4405653936073));
#16895=CARTESIAN_POINT('Ctrl Pts',(17.2858341932194,9.77439024390244,-18.4545876051966));
#16896=CARTESIAN_POINT('Origin',(16.4780203712883,9.75,-17.8656547184365));
#16897=CARTESIAN_POINT('Ctrl Pts',(16.478020371287,10.75,-17.8656547184383));
#16898=CARTESIAN_POINT('Ctrl Pts',(17.2666005307932,10.75,-18.4405653935993));
#16899=CARTESIAN_POINT('Ctrl Pts',(17.2858341932202,9.77439024390244,-18.4545876051886));
#16900=CARTESIAN_POINT('Ctrl Pts',(17.0876217955002,10.75,-17.0294907556147));
#16901=CARTESIAN_POINT('Ctrl Pts',(17.8730318351501,10.75,-17.6235351385526));
#16902=CARTESIAN_POINT('Ctrl Pts',(17.8824917699869,9.76550892532975,-17.6365459729653));
#16903=CARTESIAN_POINT('Ctrl Pts',(17.7244639958765,10.75,-16.2146287497473));
#16904=CARTESIAN_POINT('Ctrl Pts',(18.5021835427756,10.75,-16.8319676033442));
#16905=CARTESIAN_POINT('Ctrl Pts',(18.505450860094,9.75743449038534,-16.8395985788126));
#16906=CARTESIAN_POINT('Ctrl Pts',(18.3893975112944,10.75,-15.4217398231068));
#16907=CARTESIAN_POINT('Ctrl Pts',(19.1556224075984,10.75,-16.0643123157362));
#16908=CARTESIAN_POINT('Ctrl Pts',(19.1556224075984,9.75,-16.0643123157362));
#16909=CARTESIAN_POINT('Origin',(18.3893975112944,9.75,-15.4217398231068));
#16910=CARTESIAN_POINT('Origin',(0.,9.75,0.));
#16911=CARTESIAN_POINT('Origin',(-18.3893975112961,9.75,-15.4217398231048));
#16912=CARTESIAN_POINT('Ctrl Pts',(-18.3893975112962,10.75,-15.4217398231047));
#16913=CARTESIAN_POINT('Ctrl Pts',(-19.1556224076002,10.75,-16.0643123157342));
#16914=CARTESIAN_POINT('Ctrl Pts',(-19.1556224076001,9.74999999999998,-16.0643123157342));
#16915=CARTESIAN_POINT('Ctrl Pts',(-17.7244639958755,10.75,-16.2146287497338));
#16916=CARTESIAN_POINT('Ctrl Pts',(-18.5021835427609,10.75,-16.831967603351));
#16917=CARTESIAN_POINT('Ctrl Pts',(-18.5054508600983,9.75743449038528,-16.8395985788073));
#16918=CARTESIAN_POINT('Ctrl Pts',(-17.087621795494,10.75,-17.0294907555989));
#16919=CARTESIAN_POINT('Ctrl Pts',(-17.8730318353239,10.75,-17.6235351386475));
#16920=CARTESIAN_POINT('Ctrl Pts',(-17.882491769997,9.76550892511712,-17.636545972961));
#16921=CARTESIAN_POINT('Ctrl Pts',(-16.4780203712963,10.75,-17.8656547184255));
#16922=CARTESIAN_POINT('Ctrl Pts',(-17.2666005308023,10.75,-18.4405653935868));
#16923=CARTESIAN_POINT('Ctrl Pts',(-17.2858341932293,9.77439024390244,-18.4545876051761));
#16924=CARTESIAN_POINT('Origin',(-16.4780203712963,9.75,-17.8656547184255));
#16925=CARTESIAN_POINT('Ctrl Pts',(-16.4780203712963,10.75,-17.8656547184255));
#16926=CARTESIAN_POINT('Ctrl Pts',(-17.2666005308023,10.75,-18.4405653935868));
#16927=CARTESIAN_POINT('Ctrl Pts',(-17.2858341932293,9.77439024390244,-18.4545876051761));
#16928=CARTESIAN_POINT('Ctrl Pts',(-16.4201864022648,10.75,-17.9449830848021));
#16929=CARTESIAN_POINT('Ctrl Pts',(-17.1646987552868,10.75,-18.5014815360729));
#16930=CARTESIAN_POINT('Ctrl Pts',(-17.218866142633,9.82303803510935,-18.5444300755103));
#16931=CARTESIAN_POINT('Ctrl Pts',(-16.3609340347869,10.75,-18.02263898301));
#16932=CARTESIAN_POINT('Ctrl Pts',(-17.0565699547838,10.75,-18.5602973050011));
#16933=CARTESIAN_POINT('Ctrl Pts',(-17.1454229102227,9.87836276842072,-18.6315395728606));
#16934=CARTESIAN_POINT('Ctrl Pts',(-16.2394647608977,10.75,-18.1745295246669));
#16935=CARTESIAN_POINT('Ctrl Pts',(-16.8540047055406,10.75,-18.6788326359793));
#16936=CARTESIAN_POINT('Ctrl Pts',(-16.9922413943597,9.97582686527399,-18.7950045725024));
#16937=CARTESIAN_POINT('Ctrl Pts',(-16.1773081113176,10.75,-18.2488221735804));
#16938=CARTESIAN_POINT('Ctrl Pts',(-16.7583976671095,10.75,-18.7391027373331));
#16939=CARTESIAN_POINT('Ctrl Pts',(-16.9133187470158,10.0176700000194,-18.8718344001161));
#16940=CARTESIAN_POINT('Ctrl Pts',(-15.9875644144501,10.75,-18.4678954650287));
#16941=CARTESIAN_POINT('Ctrl Pts',(-16.4909861673416,10.75,-18.9187569933661));
#16942=CARTESIAN_POINT('Ctrl Pts',(-16.6765372063045,10.1240114260742,-19.0935506433102));
#16943=CARTESIAN_POINT('Ctrl Pts',(-15.8568225101403,10.75,-18.6090096240717));
#16944=CARTESIAN_POINT('Ctrl Pts',(-16.3229486004107,10.75,-19.0436478681489));
#16945=CARTESIAN_POINT('Ctrl Pts',(-16.5179814662747,10.1729273502797,-19.2306007925839));
#16946=CARTESIAN_POINT('Ctrl Pts',(-15.4560570391986,10.75,-19.022427441684));
#16947=CARTESIAN_POINT('Ctrl Pts',(-15.8403045574767,10.75,-19.4059080219932));
#16948=CARTESIAN_POINT('Ctrl Pts',(-16.0415174065673,10.2970310354252,-19.6286372648663));
#16949=CARTESIAN_POINT('Ctrl Pts',(-15.1775121139771,10.75,-19.2848278240086));
#16950=CARTESIAN_POINT('Ctrl Pts',(-15.5212812150538,10.75,-19.6505377189946));
#16951=CARTESIAN_POINT('Ctrl Pts',(-15.7216572711263,10.348875402469,-19.8754301022878));
#16952=CARTESIAN_POINT('Ctrl Pts',(-14.3174283733606,10.75,-20.0436150917647));
#16953=CARTESIAN_POINT('Ctrl Pts',(-14.5807052024803,10.75,-20.3431259159971));
#16954=CARTESIAN_POINT('Ctrl Pts',(-14.7498205235984,10.4800501520585,-20.5861008531739));
#16955=CARTESIAN_POINT('Ctrl Pts',(-13.7112218641341,10.75,-20.5113338976033));
#16956=CARTESIAN_POINT('Ctrl Pts',(-13.9284252757989,10.7499999999993,-20.7911770990046));
#16957=CARTESIAN_POINT('Ctrl Pts',(-14.0859782414491,10.5295463004092,-21.0183499982884));
#16958=CARTESIAN_POINT('Ctrl Pts',(-12.4444282590142,10.75,-21.3835719658861));
#16959=CARTESIAN_POINT('Ctrl Pts',(-12.5993509724761,10.7500000000007,-21.6142534710497));
#16960=CARTESIAN_POINT('Ctrl Pts',(-12.7203223126449,10.6086489117022,-21.8215270095887));
#16961=CARTESIAN_POINT('Ctrl Pts',(-11.7822109370075,10.75,-21.7877736287786));
#16962=CARTESIAN_POINT('Ctrl Pts',(-11.9106547115054,10.75,-21.9998133945471));
#16963=CARTESIAN_POINT('Ctrl Pts',(-12.0175682524596,10.6355424608076,-22.1915948020202));
#16964=CARTESIAN_POINT('Ctrl Pts',(-10.4276042052731,10.75,-22.5220998589761));
#16965=CARTESIAN_POINT('Ctrl Pts',(-10.517968550615,10.75,-22.6958229564086));
#16966=CARTESIAN_POINT('Ctrl Pts',(-10.5948532243925,10.6772804141949,-22.8609639240628));
#16967=CARTESIAN_POINT('Ctrl Pts',(-9.73251018538841,10.75,-22.8541153700753));
#16968=CARTESIAN_POINT('Ctrl Pts',(-9.80642247244996,10.7500000000007,-23.0117088133774));
#16969=CARTESIAN_POINT('Ctrl Pts',(-9.87204995901313,10.6919698658189,-23.1619487822281));
#16970=CARTESIAN_POINT('Ctrl Pts',(-7.5953935489335,10.75,-23.7477563831789));
#16971=CARTESIAN_POINT('Ctrl Pts',(-7.63899237204751,10.7499999999987,-23.8550327052981));
#16972=CARTESIAN_POINT('Ctrl Pts',(-7.66543048576834,10.7263148678275,-23.9669915332266));
#16973=CARTESIAN_POINT('Ctrl Pts',(-6.11513874037353,10.75,-24.2011081296453));
#16974=CARTESIAN_POINT('Ctrl Pts',(-6.13861428588092,10.7500000000081,-24.2845436650569));
#16975=CARTESIAN_POINT('Ctrl Pts',(-6.15722358267897,10.7363628565299,-24.3678462428209));
#16976=CARTESIAN_POINT('Ctrl Pts',(-3.08771028814254,10.75,-24.8194092303953));
#16977=CARTESIAN_POINT('Ctrl Pts',(-3.09355332608735,10.749999999992,-24.8560196583291));
#16978=CARTESIAN_POINT('Ctrl Pts',(-3.09482729538221,10.7484649507037,-24.8935813777596));
#16979=CARTESIAN_POINT('Ctrl Pts',(-1.54655171301441,10.75,-24.9814490354507));
#16980=CARTESIAN_POINT('Ctrl Pts',(-1.54684319067547,10.75,-24.998560764468));
#16981=CARTESIAN_POINT('Ctrl Pts',(-1.54703957001513,10.75,-25.0156741336263));
#16982=CARTESIAN_POINT('Ctrl Pts',(6.05752864795171E-16,10.75,-25.));
#16983=CARTESIAN_POINT('Ctrl Pts',(6.05752864795171E-16,10.75,-25.));
#16984=CARTESIAN_POINT('Ctrl Pts',(6.05752864795171E-16,10.75,-25.));
#16985=CARTESIAN_POINT('Origin',(0.,-1.42723068592072E-14,-61.5));
#16986=CARTESIAN_POINT('',(-10.7,-1.31037207508767E-15,-61.5));
#16987=CARTESIAN_POINT('Origin',(0.,0.,-61.5));
#16988=CARTESIAN_POINT('Origin',(0.,0.,0.));
#16989=CARTESIAN_POINT('',(-8.35,-1.02258007728804E-15,-63.85));
#16990=CARTESIAN_POINT('Origin',(0.,0.,-63.85));
#16991=CARTESIAN_POINT('',(-8.35,-1.02258007728804E-15,-70.75));
#16992=CARTESIAN_POINT('',(-8.35,-1.02258007728804E-15,0.));
#16993=CARTESIAN_POINT('Origin',(0.,0.,-70.75));
#16994=CARTESIAN_POINT('Ctrl Pts',(-8.35,0.,-78.75));
#16995=CARTESIAN_POINT('Ctrl Pts',(-8.35,-8.35,-78.75));
#16996=CARTESIAN_POINT('Ctrl Pts',(0.,-8.35,-78.75));
#16997=CARTESIAN_POINT('Ctrl Pts',(8.35,-8.35,-78.75));
#16998=CARTESIAN_POINT('Ctrl Pts',(8.35,0.,-78.75));
#16999=CARTESIAN_POINT('Ctrl Pts',(8.35,8.35,-78.75));
#17000=CARTESIAN_POINT('Ctrl Pts',(0.,8.35,-78.75));
#17001=CARTESIAN_POINT('Ctrl Pts',(-8.35,8.35,-78.75));
#17002=CARTESIAN_POINT('Ctrl Pts',(-8.35,0.,-78.75));
#17003=CARTESIAN_POINT('Ctrl Pts',(-10.2459842001317,0.,-74.75));
#17004=CARTESIAN_POINT('Ctrl Pts',(-10.2459842001317,-10.2459842001317,
-74.75));
#17005=CARTESIAN_POINT('Ctrl Pts',(0.,-10.2459842001317,-74.75));
#17006=CARTESIAN_POINT('Ctrl Pts',(10.2459842001317,-10.2459842001317,-74.75));
#17007=CARTESIAN_POINT('Ctrl Pts',(10.2459842001317,0.,-74.75));
#17008=CARTESIAN_POINT('Ctrl Pts',(10.2459842001317,10.2459842001317,-74.75));
#17009=CARTESIAN_POINT('Ctrl Pts',(0.,10.2459842001317,-74.75));
#17010=CARTESIAN_POINT('Ctrl Pts',(-10.2459842001317,10.2459842001317,-74.75));
#17011=CARTESIAN_POINT('Ctrl Pts',(-10.2459842001317,0.,-74.75));
#17012=CARTESIAN_POINT('Ctrl Pts',(-8.35,0.,-70.75));
#17013=CARTESIAN_POINT('Ctrl Pts',(-8.35,-8.35,-70.75));
#17014=CARTESIAN_POINT('Ctrl Pts',(0.,-8.35,-70.75));
#17015=CARTESIAN_POINT('Ctrl Pts',(8.35,-8.35,-70.75));
#17016=CARTESIAN_POINT('Ctrl Pts',(8.35,0.,-70.75));
#17017=CARTESIAN_POINT('Ctrl Pts',(8.35,8.35,-70.75));
#17018=CARTESIAN_POINT('Ctrl Pts',(0.,8.35,-70.75));
#17019=CARTESIAN_POINT('Ctrl Pts',(-8.35,8.35,-70.75));
#17020=CARTESIAN_POINT('Ctrl Pts',(-8.35,0.,-70.75));
#17021=CARTESIAN_POINT('',(-8.35,-1.02258007728804E-15,-78.75));
#17022=CARTESIAN_POINT('Origin',(0.0888888888889092,1.08857493257567E-17,
-74.75));
#17023=CARTESIAN_POINT('Origin',(0.,0.,-78.75));
#17024=CARTESIAN_POINT('',(-1.72045318260168,-8.718775769933,-77.3287673114253));
#17025=CARTESIAN_POINT('',(-3.7964050773568E-16,-8.72047257416007,-77.85));
#17026=CARTESIAN_POINT('Ctrl Pts',(-1.72045318260167,-8.718775769933,-77.3287673114253));
#17027=CARTESIAN_POINT('Ctrl Pts',(-1.65539500148226,-8.71890290462215,
-77.3721715977544));
#17028=CARTESIAN_POINT('Ctrl Pts',(-1.5891103189426,-8.71902546830415,-77.4128415044279));
#17029=CARTESIAN_POINT('Ctrl Pts',(-1.52164394658355,-8.7191425346816,-77.450851661944));
#17030=CARTESIAN_POINT('Ctrl Pts',(-1.45352593448909,-8.71926073177204,
-77.4892289494557));
#17031=CARTESIAN_POINT('Ctrl Pts',(-1.38420266457374,-8.71937332485106,
-77.5248953093588));
#17032=CARTESIAN_POINT('Ctrl Pts',(-1.31368631099614,-8.71947936052059,
-77.557886799054));
#17033=CARTESIAN_POINT('Ctrl Pts',(-1.27115196980953,-8.71954331954735,
-77.5777867400996));
#17034=CARTESIAN_POINT('Ctrl Pts',(-1.22818293533589,-8.71960489278511,
-77.5967126611893));
#17035=CARTESIAN_POINT('Ctrl Pts',(-1.18477749668439,-8.71966387100391,
-77.6146644277036));
#17036=CARTESIAN_POINT('Ctrl Pts',(-1.12217096659324,-8.71974893918303,
-77.6405574458457));
#17037=CARTESIAN_POINT('Ctrl Pts',(-1.05842838941658,-8.71982876080258,
-77.6645122082305));
#17038=CARTESIAN_POINT('Ctrl Pts',(-0.993822322159884,-8.71990251193502,
-77.6863782440239));
#17039=CARTESIAN_POINT('Ctrl Pts',(-0.929270656109259,-8.7199762009657,
-77.7082258676345));
#17040=CARTESIAN_POINT('Ctrl Pts',(-0.863857416050902,-8.72004382972822,
-77.7279880699753));
#17041=CARTESIAN_POINT('Ctrl Pts',(-0.797874747322811,-8.72010457637465,
-77.7455626996584));
#17042=CARTESIAN_POINT('Ctrl Pts',(-0.733027140671185,-8.7201642780313,
-77.7628350030482));
#17043=CARTESIAN_POINT('Ctrl Pts',(-0.667630028539082,-8.72021733231349,
-77.7779943689607));
#17044=CARTESIAN_POINT('Ctrl Pts',(-0.601973102197269,-8.7202629590612,
-77.7909913489241));
#17045=CARTESIAN_POINT('Ctrl Pts',(-0.524757209733025,-8.72031661844249,
-77.8062764599265));
#17046=CARTESIAN_POINT('Ctrl Pts',(-0.447291752022074,-8.72036016052982,
-77.8185591941));
#17047=CARTESIAN_POINT('Ctrl Pts',(-0.369584773909021,-8.72039335911026,
-77.8278900394418));
#17048=CARTESIAN_POINT('Ctrl Pts',(-0.291661027798569,-8.72042665030001,
-77.8372469137028));
#17049=CARTESIAN_POINT('Ctrl Pts',(-0.213493632636301,-8.72044954019479,
-77.8436355249856));
#17050=CARTESIAN_POINT('Ctrl Pts',(-0.135080649621019,-8.72046180068327,
-77.8470555723296));
#17051=CARTESIAN_POINT('Ctrl Pts',(-0.0901346875977141,-8.720468828339,
-77.8490159277725));
#17052=CARTESIAN_POINT('Ctrl Pts',(-0.0451079148060559,-8.72047236367163,
-77.85));
#17053=CARTESIAN_POINT('Ctrl Pts',(-3.7964050773568E-16,-8.72047236372208,
-77.85));
#17054=CARTESIAN_POINT('Ctrl Pts',(-3.7964050773568E-16,-8.72047236372208,
-77.85));
#17055=CARTESIAN_POINT('Ctrl Pts',(0.000299910886524944,-8.72047236372241,
-77.85));
#17056=CARTESIAN_POINT('Ctrl Pts',(0.000599825357673861,-8.72047236356647,
-77.8499999564775));
#17057=CARTESIAN_POINT('Ctrl Pts',(0.000899743413439149,-8.72047236325423,
-77.8499998694293));
#17058=CARTESIAN_POINT('Ctrl Pts',(0.0640429304707948,-8.72047229751748,
-77.8499815427619));
#17059=CARTESIAN_POINT('Ctrl Pts',(0.127461864754973,-8.7204650795781,-77.8480295862201));
#17060=CARTESIAN_POINT('Ctrl Pts',(0.190853933637923,-8.72045096523215,
-77.844119386193));
#17061=CARTESIAN_POINT('Ctrl Pts',(0.254193326196229,-8.72043686261466,
-77.8402124353888));
#17062=CARTESIAN_POINT('Ctrl Pts',(0.317505410088621,-8.72041587504713,
-77.8343504951573));
#17063=CARTESIAN_POINT('Ctrl Pts',(0.380489429511035,-8.72038825768846,
-77.8265610336918));
#17064=CARTESIAN_POINT('Ctrl Pts',(0.443564297220783,-8.72036060049445,
-77.81876033669));
#17065=CARTESIAN_POINT('Ctrl Pts',(0.506309670583462,-8.72032629436986,
-77.8090266361057));
#17066=CARTESIAN_POINT('Ctrl Pts',(0.56843190743774,-8.72028559557932,-77.7974391161444));
#17067=CARTESIAN_POINT('Ctrl Pts',(0.581380258335366,-8.72027711259082,
-77.7950238896154));
#17068=CARTESIAN_POINT('Ctrl Pts',(0.594301580864125,-8.72026835187617,
-77.7925283002156));
#17069=CARTESIAN_POINT('Ctrl Pts',(0.607193291675441,-8.72025931575594,
-77.7899533395341));
#17070=CARTESIAN_POINT('Ctrl Pts',(0.684092206541919,-8.72020541539694,
-77.7745937270569));
#17071=CARTESIAN_POINT('Ctrl Pts',(0.76023810077427,-8.72014184272655,-77.7563546896797));
#17072=CARTESIAN_POINT('Ctrl Pts',(0.835637247932075,-8.72006925722806,
-77.7352487986546));
#17073=CARTESIAN_POINT('Ctrl Pts',(0.910709368037719,-8.71999698655304,
-77.7142344497434));
#17074=CARTESIAN_POINT('Ctrl Pts',(0.985041941757664,-8.71991578106266,
-77.6903778171793));
#17075=CARTESIAN_POINT('Ctrl Pts',(1.05862557413108,-8.71982629169629,-77.6636423757551));
#17076=CARTESIAN_POINT('Ctrl Pts',(1.1017309535722,-8.71977386871893,-77.6479807223419));
#17077=CARTESIAN_POINT('Ctrl Pts',(1.14457897534976,-8.71971860302155,-77.6313302639057));
#17078=CARTESIAN_POINT('Ctrl Pts',(1.18716371754352,-8.71966062545943,-77.6136763622568));
#17079=CARTESIAN_POINT('Ctrl Pts',(1.26405807871352,-8.71955593661147,-77.5817990883903));
#17080=CARTESIAN_POINT('Ctrl Pts',(1.33962433782053,-8.71944296612345,-77.5468383309899));
#17081=CARTESIAN_POINT('Ctrl Pts',(1.41354178114807,-8.7193235640821,-77.5089671315456));
#17082=CARTESIAN_POINT('Ctrl Pts',(1.48753950477095,-8.71920403236052,-77.4710548009292));
#17083=CARTESIAN_POINT('Ctrl Pts',(1.55988439051607,-8.71907805510766,-77.4302259909402));
#17084=CARTESIAN_POINT('Ctrl Pts',(1.63028320823959,-8.71894748844484,-77.3866980602511));
#17085=CARTESIAN_POINT('Ctrl Pts',(1.66176045181976,-8.71888910850635,-77.3672355277663));
#17086=CARTESIAN_POINT('Ctrl Pts',(1.69284905171952,-8.71882981103946,-77.3472339354576));
#17087=CARTESIAN_POINT('Ctrl Pts',(1.72352497634196,-8.71876976196479,-77.3267152842186));
#17088=CARTESIAN_POINT('Ctrl Pts',(1.80027708010235,-8.7186195173392,-77.2753769898296));
#17089=CARTESIAN_POINT('Ctrl Pts',(1.87496173999789,-8.71846358768554,-77.2204528708162));
#17090=CARTESIAN_POINT('Ctrl Pts',(1.94719992345561,-8.71830462487999,-77.1621385652766));
#17091=CARTESIAN_POINT('Ctrl Pts',(2.01930828703512,-8.71814594774791,-77.103929056891));
#17092=CARTESIAN_POINT('Ctrl Pts',(2.0889785347496,-8.71798424835595,-77.0423417416205));
#17093=CARTESIAN_POINT('Ctrl Pts',(2.15585718417934,-8.71782216430884,-76.9776175168602));
#17094=CARTESIAN_POINT('Ctrl Pts',(2.16846973129543,-8.7177915971144,-76.9654112695555));
#17095=CARTESIAN_POINT('Ctrl Pts',(2.18098307120848,-8.71776101623946,-76.9530935832101));
#17096=CARTESIAN_POINT('Ctrl Pts',(2.19339494574377,-8.71773043937514,-76.9406662484244));
#17097=CARTESIAN_POINT('Ctrl Pts',(2.24888782190004,-8.71759373172956,-76.8851042502544));
#17098=CARTESIAN_POINT('Ctrl Pts',(2.30197065297182,-8.71745811411991,-76.8277389943072));
#17099=CARTESIAN_POINT('Ctrl Pts',(2.35269578179276,-8.71732466077813,-76.7686189730444));
#17100=CARTESIAN_POINT('Ctrl Pts',(2.4037590828821,-8.71719031773492,-76.7091048127786));
#17101=CARTESIAN_POINT('Ctrl Pts',(2.45243369256433,-8.71705816791309,-76.6478118562424));
#17102=CARTESIAN_POINT('Ctrl Pts',(2.49873800210765,-8.71692930717307,-76.584750227367));
#17103=CARTESIAN_POINT('Ctrl Pts',(2.52592884079295,-8.716853637508,-76.547719147649));
#17104=CARTESIAN_POINT('Ctrl Pts',(2.55230163167014,-8.71677910201007,-76.5100774807928));
#17105=CARTESIAN_POINT('Ctrl Pts',(2.57785340962773,-8.71670592258005,-76.4718222319597));
#17106=CARTESIAN_POINT('Ctrl Pts',(2.61310530671562,-8.71660496233609,-76.4190442962256));
#17107=CARTESIAN_POINT('Ctrl Pts',(2.64690716808691,-8.71650634668673,-76.3649202782147));
#17108=CARTESIAN_POINT('Ctrl Pts',(2.67906408116098,-8.71641099671277,-76.3096844709854));
#17109=CARTESIAN_POINT('Ctrl Pts',(2.71118233434677,-8.71631576137105,-76.2545150696992));
#17110=CARTESIAN_POINT('Ctrl Pts',(2.74165931100356,-8.71622378385729,-76.1982369517102));
#17111=CARTESIAN_POINT('Ctrl Pts',(2.77034413004262,-8.71613598193422,-76.1411122891911));
#17112=CARTESIAN_POINT('Ctrl Pts',(2.79905294328358,-8.71604810656682,-76.0839398431847));
#17113=CARTESIAN_POINT('Ctrl Pts',(2.82596638926419,-8.71596441377862,-76.0259198799202));
#17114=CARTESIAN_POINT('Ctrl Pts',(2.85098035509833,-8.71588582363734,-75.9673376749462));
#17115=CARTESIAN_POINT('Ctrl Pts',(2.85565776855165,-8.7158711279035,-75.9563832666973));
#17116=CARTESIAN_POINT('Ctrl Pts',(2.86026890187996,-8.71585661058901,-75.9454092510284));
#17117=CARTESIAN_POINT('Ctrl Pts',(2.86481326500262,-8.7158422777096,-75.9344175600966));
#17118=CARTESIAN_POINT('Ctrl Pts',(2.89487646954094,-8.71574745863955,-75.8617021005733));
#17119=CARTESIAN_POINT('Ctrl Pts',(2.92207389877206,-8.71566033761335,-75.7880886511198));
#17120=CARTESIAN_POINT('Ctrl Pts',(2.94643811869778,-8.71558151593588,-75.7135883004088));
#17121=CARTESIAN_POINT('Ctrl Pts',(2.9707918943071,-8.71550272804726,-75.639119886088));
#17122=CARTESIAN_POINT('Ctrl Pts',(2.99231512996288,-8.71543223239345,-75.5637645823351));
#17123=CARTESIAN_POINT('Ctrl Pts',(3.01099152146986,-8.71537062950641,-75.487516140594));
#17124=CARTESIAN_POINT('Ctrl Pts',(3.02176016915483,-8.71533510980836,-75.4435519409075));
#17125=CARTESIAN_POINT('Ctrl Pts',(3.03158143712092,-8.71530254657911,-75.3992905484563));
#17126=CARTESIAN_POINT('Ctrl Pts',(3.0404443852463,-8.71527305493598,-75.354729642257));
#17127=CARTESIAN_POINT('Ctrl Pts',(3.05342506233143,-8.71522986146461,-75.2894657226435));
#17128=CARTESIAN_POINT('Ctrl Pts',(3.06433888891931,-8.71519347811349,-75.2235881046905));
#17129=CARTESIAN_POINT('Ctrl Pts',(3.07311393468772,-8.71516409033977,-75.1573950716788));
#17130=CARTESIAN_POINT('Ctrl Pts',(3.08211546594833,-8.71513394406239,-75.0894935847106));
#17131=CARTESIAN_POINT('Ctrl Pts',(3.08886606565568,-8.71511115913683,-75.0212606998728));
#17132=CARTESIAN_POINT('Ctrl Pts',(3.09334449590245,-8.71509593575412,-74.9530266723119));
#17133=CARTESIAN_POINT('Ctrl Pts',(3.09782292614922,-8.71508071237141,-74.884792644751));
#17134=CARTESIAN_POINT('Ctrl Pts',(3.10002921243779,-8.71507305053155,-74.8165580440902));
#17135=CARTESIAN_POINT('Ctrl Pts',(3.09999970736836,-8.71507315042558,-74.74865303448));
#17136=CARTESIAN_POINT('Ctrl Pts',(3.0999658079665,-8.71507326519731,-74.6706346039406));
#17137=CARTESIAN_POINT('Ctrl Pts',(3.09699103187926,-8.71508334203519,-74.592719406739));
#17138=CARTESIAN_POINT('Ctrl Pts',(3.09107242805617,-8.71510332750266,-74.514901628013));
#17139=CARTESIAN_POINT('Ctrl Pts',(3.08519738465212,-8.7151231658788,-74.4376565814973));
#17140=CARTESIAN_POINT('Ctrl Pts',(3.07642156717969,-8.71515276756792,-74.3605067705524));
#17141=CARTESIAN_POINT('Ctrl Pts',(3.06469171994945,-8.7151920803047,-74.2834545449012));
#17142=CARTESIAN_POINT('Ctrl Pts',(3.05764210342273,-8.71521570718691,-74.2371462995585));
#17143=CARTESIAN_POINT('Ctrl Pts',(3.04952453053919,-8.7152428416877,-74.1908735071733));
#17144=CARTESIAN_POINT('Ctrl Pts',(3.04031890638674,-8.7152734724613,-74.1446398200514));
#17145=CARTESIAN_POINT('Ctrl Pts',(3.02312760546873,-8.71533067475824,-74.0582994247997));
#17146=CARTESIAN_POINT('Ctrl Pts',(3.00236130986795,-8.71539936732086,-73.9731867127046));
#17147=CARTESIAN_POINT('Ctrl Pts',(2.97813906776938,-8.71547848786435,-73.8893678526654));
#17148=CARTESIAN_POINT('Ctrl Pts',(2.95358359569693,-8.71555869688413,-73.8043958806876));
#17149=CARTESIAN_POINT('Ctrl Pts',(2.92547631861943,-8.7156496227778,-73.7207526603851));
#17150=CARTESIAN_POINT('Ctrl Pts',(2.89388813158801,-8.71575015881243,-73.6385093424351));
#17151=CARTESIAN_POINT('Ctrl Pts',(2.88421919183921,-8.7157809322424,-73.6133351947321));
#17152=CARTESIAN_POINT('Ctrl Pts',(2.87422375058271,-8.71581260607772,-73.5882922788232));
#17153=CARTESIAN_POINT('Ctrl Pts',(2.8639029002749,-8.7158451485785,-73.5633828849216));
#17154=CARTESIAN_POINT('Ctrl Pts',(2.83722639600753,-8.71592926181869,-73.4989990858261));
#17155=CARTESIAN_POINT('Ctrl Pts',(2.80825858386043,-8.71601965988724,-73.4352360891271));
#17156=CARTESIAN_POINT('Ctrl Pts',(2.77708668903123,-8.71611528859754,-73.3723971829277));
#17157=CARTESIAN_POINT('Ctrl Pts',(2.7459426515262,-8.71621083184751,-73.3096144338464));
#17158=CARTESIAN_POINT('Ctrl Pts',(2.71259864889984,-8.71631159639449,-73.247754606431));
#17159=CARTESIAN_POINT('Ctrl Pts',(2.67718998623632,-8.71641653087558,-73.1871008421539));
#17160=CARTESIAN_POINT('Ctrl Pts',(2.6453452533964,-8.71651090355912,-73.1325519613478));
#17161=CARTESIAN_POINT('Ctrl Pts',(2.6118313261885,-8.71660864900209,-73.0789785513262));
#17162=CARTESIAN_POINT('Ctrl Pts',(2.57677782571062,-8.71670900242383,-73.0265685285089));
#17163=CARTESIAN_POINT('Ctrl Pts',(2.53302624838245,-8.71683425726091,-72.9611536302875));
#17164=CARTESIAN_POINT('Ctrl Pts',(2.48698488900056,-8.71696313162736,-72.8976977641212));
#17165=CARTESIAN_POINT('Ctrl Pts',(2.43869838176886,-8.7170944992703,-72.8361687109993));
#17166=CARTESIAN_POINT('Ctrl Pts',(2.39024128370483,-8.71722633102043,-72.7744222826108));
#17167=CARTESIAN_POINT('Ctrl Pts',(2.33952268394173,-8.7173606736951,-72.7146156676716));
#17168=CARTESIAN_POINT('Ctrl Pts',(2.28654394533952,-8.71749638906238,-72.6567449304896));
#17169=CARTESIAN_POINT('Ctrl Pts',(2.25591502933889,-8.71757485100191,-72.6232877739998));
#17170=CARTESIAN_POINT('Ctrl Pts',(2.22452990562365,-8.71765377175192,-72.5904782499961));
#17171=CARTESIAN_POINT('Ctrl Pts',(2.19238316845143,-8.71773293136402,-72.5583211816758));
#17172=CARTESIAN_POINT('Ctrl Pts',(2.14794006336032,-8.71784237012106,-72.5138637936951));
#17173=CARTESIAN_POINT('Ctrl Pts',(2.10193823605173,-8.71795248897054,-72.4705578338053));
#17174=CARTESIAN_POINT('Ctrl Pts',(2.05457270333021,-8.71806216059154,-72.4286359598869));
#17175=CARTESIAN_POINT('Ctrl Pts',(2.00725118285122,-8.71817173030522,-72.3867530399415));
#17176=CARTESIAN_POINT('Ctrl Pts',(1.958568832385,-8.71828085362116,-72.3462519807932));
#17177=CARTESIAN_POINT('Ctrl Pts',(1.90875629780346,-8.71838840635804,-72.3073274072042));
#17178=CARTESIAN_POINT('Ctrl Pts',(1.85887614986205,-8.71849610508231,-72.2683499990983));
#17179=CARTESIAN_POINT('Ctrl Pts',(1.8078631442273,-8.71860222896096,-72.2309536442723));
#17180=CARTESIAN_POINT('Ctrl Pts',(1.75597961225169,-8.71870564922871,-72.1952914840717));
#17181=CARTESIAN_POINT('Ctrl Pts',(1.7444829025098,-8.7187285658027,-72.1873892174183));
#17182=CARTESIAN_POINT('Ctrl Pts',(1.73294355506966,-8.71875134962739,-72.1795719277208));
#17183=CARTESIAN_POINT('Ctrl Pts',(1.72136459638604,-8.71877398842172,-72.1718409811828));
#17184=CARTESIAN_POINT('Ctrl Pts',(1.65608855780722,-8.71890161395805,-72.1282579977509));
#17185=CARTESIAN_POINT('Ctrl Pts',(1.58931917610361,-8.71902518049889,-72.0872569224723));
#17186=CARTESIAN_POINT('Ctrl Pts',(1.52106342354734,-8.71914358262926,-72.0488213569728));
#17187=CARTESIAN_POINT('Ctrl Pts',(1.45305348802619,-8.71926155834487,-72.0105242137512));
#17188=CARTESIAN_POINT('Ctrl Pts',(1.38356717504495,-8.71937440678136,-71.9747737795834));
#17189=CARTESIAN_POINT('Ctrl Pts',(1.31258722743462,-8.71948103442396,-71.9415992503962));
#17190=CARTESIAN_POINT('Ctrl Pts',(1.27119052763988,-8.7195432214593,-71.9222513067609));
#17191=CARTESIAN_POINT('Ctrl Pts',(1.22928537930285,-8.7196032925422,-71.903780415527));
#17192=CARTESIAN_POINT('Ctrl Pts',(1.18686599705147,-8.71966103074505,-71.8862002330744));
#17193=CARTESIAN_POINT('Ctrl Pts',(1.11536548171387,-8.71975835208826,-71.8565677387199));
#17194=CARTESIAN_POINT('Ctrl Pts',(1.04272571061629,-8.7198484073864,-71.8296054502696));
#17195=CARTESIAN_POINT('Ctrl Pts',(0.969264783005578,-8.71993024967823,
-71.8054243462894));
#17196=CARTESIAN_POINT('Ctrl Pts',(0.895724679176382,-8.72001218017971,
-71.7812171799052));
#17197=CARTESIAN_POINT('Ctrl Pts',(0.821362159731487,-8.72008587996139,
-71.7597973336574));
#17198=CARTESIAN_POINT('Ctrl Pts',(0.746509800824368,-8.72015039899682,
-71.7412256453378));
#17199=CARTESIAN_POINT('Ctrl Pts',(0.699376616873181,-8.72019102547285,
-71.7295313872725));
#17200=CARTESIAN_POINT('Ctrl Pts',(0.652049454415536,-8.72022801178817,
-71.7189654010855));
#17201=CARTESIAN_POINT('Ctrl Pts',(0.604612671139789,-8.72026112075105,
-71.7095323521048));
#17202=CARTESIAN_POINT('Ctrl Pts',(0.492199602444168,-8.7203395805424,-71.6871784336929));
#17203=CARTESIAN_POINT('Ctrl Pts',(0.378251973714541,-8.72039706472714,
-71.671003936024));
#17204=CARTESIAN_POINT('Ctrl Pts',(0.263380851782798,-8.72043208706923,
-71.6612088890775));
#17205=CARTESIAN_POINT('Ctrl Pts',(0.175897227641158,-8.72045875940742,
-71.65374917082));
#17206=CARTESIAN_POINT('Ctrl Pts',(0.0878785715260265,-8.72047240376249,
-71.6499888373265));
#17207=CARTESIAN_POINT('Ctrl Pts',(-0.000392895601461571,-8.72047236363328,
-71.6500000248979));
#17208=CARTESIAN_POINT('Ctrl Pts',(-0.0788581112235056,-8.72047232796211,
-71.6500099696199));
#17209=CARTESIAN_POINT('Ctrl Pts',(-0.156878976850864,-8.72046160079282,
-71.6529946419127));
#17210=CARTESIAN_POINT('Ctrl Pts',(-0.234458459311995,-8.72044056033218,
-71.6588789685849));
#17211=CARTESIAN_POINT('Ctrl Pts',(-0.312611281100131,-8.72041936437522,
-71.6648067824754));
#17212=CARTESIAN_POINT('Ctrl Pts',(-0.390316953274498,-8.72038770212602,
-71.6736772639242));
#17213=CARTESIAN_POINT('Ctrl Pts',(-0.46758220711631,-8.72034596023869,
-71.6854662867594));
#17214=CARTESIAN_POINT('Ctrl Pts',(-0.513198175170774,-8.72032131660518,
-71.6924263064618));
#17215=CARTESIAN_POINT('Ctrl Pts',(-0.558660646769238,-8.72029315971191,
-71.7004045820686));
#17216=CARTESIAN_POINT('Ctrl Pts',(-0.603969926403656,-8.72026156912362,
-71.70940460962));
#17217=CARTESIAN_POINT('Ctrl Pts',(-0.666812925267637,-8.72021775365536,
-71.7218874547625));
#17218=CARTESIAN_POINT('Ctrl Pts',(-0.729577541050631,-8.72016698756626,
-71.7363842594945));
#17219=CARTESIAN_POINT('Ctrl Pts',(-0.791959476863296,-8.72010995703038,
-71.7528680064091));
#17220=CARTESIAN_POINT('Ctrl Pts',(-0.85426463882863,-8.72005299668235,
-71.7693314666709));
#17221=CARTESIAN_POINT('Ctrl Pts',(-0.916187576992764,-8.71998978729745,
-71.7877768974763));
#17222=CARTESIAN_POINT('Ctrl Pts',(-0.977435294335463,-8.71992101251944,
-71.8081264056069));
#17223=CARTESIAN_POINT('Ctrl Pts',(-1.03872472132528,-8.71985219090586,
-71.8284897717364));
#17224=CARTESIAN_POINT('Ctrl Pts',(-1.09933754194174,-8.71977779631652,
-71.8507596442123));
#17225=CARTESIAN_POINT('Ctrl Pts',(-1.15899751628672,-8.71969851379281,
-71.8748087442326));
#17226=CARTESIAN_POINT('Ctrl Pts',(-1.16832598893221,-8.7196861171255,-71.8785690772557));
#17227=CARTESIAN_POINT('Ctrl Pts',(-1.17763120827332,-8.71967360095478,
-71.8823728154656));
#17228=CARTESIAN_POINT('Ctrl Pts',(-1.18691216784278,-8.71966096789941,
-71.8862193684176));
#17229=CARTESIAN_POINT('Ctrl Pts',(-1.25962167120132,-8.7195619971869,-71.9163542863307));
#17230=CARTESIAN_POINT('Ctrl Pts',(-1.33092427709693,-8.71945601925101,
-71.9491461201246));
#17231=CARTESIAN_POINT('Ctrl Pts',(-1.40083655360198,-8.71934409131941,
-71.9845602609906));
#17232=CARTESIAN_POINT('Ctrl Pts',(-1.4707719340463,-8.71923212639895,-72.0199861051826));
#17233=CARTESIAN_POINT('Ctrl Pts',(-1.53931676946223,-8.71911420754953,
-72.058036343111));
#17234=CARTESIAN_POINT('Ctrl Pts',(-1.60646589924809,-8.71899139304733,
-72.0987234556627));
#17235=CARTESIAN_POINT('Ctrl Pts',(-1.64514751867028,-8.71892064508904,
-72.1221614869244));
#17236=CARTESIAN_POINT('Ctrl Pts',(-1.68336552882153,-8.71884827255814,
-72.1464753830905));
#17237=CARTESIAN_POINT('Ctrl Pts',(-1.72111430332097,-8.71877447775272,
-72.1716738850751));
#17238=CARTESIAN_POINT('Ctrl Pts',(-1.77546294501159,-8.71866823198736,
-72.2079533239088));
#17239=CARTESIAN_POINT('Ctrl Pts',(-1.82884692297603,-8.71855898012913,
-72.2460781855651));
#17240=CARTESIAN_POINT('Ctrl Pts',(-1.88100370177939,-8.71844793038841,
-72.2858926415653));
#17241=CARTESIAN_POINT('Ctrl Pts',(-1.93313773363776,-8.71833692907942,
-72.3256897334325));
#17242=CARTESIAN_POINT('Ctrl Pts',(-1.984045231546,-8.71822413145581,-72.3671746566697));
#17243=CARTESIAN_POINT('Ctrl Pts',(-2.0334946489006,-8.71811074414789,-72.4101496815197));
#17244=CARTESIAN_POINT('Ctrl Pts',(-2.08302250952138,-8.71799717696988,
-72.4531928790902));
#17245=CARTESIAN_POINT('Ctrl Pts',(-2.13108730686939,-8.7178830182352,-72.4977305567866));
#17246=CARTESIAN_POINT('Ctrl Pts',(-2.17749286533221,-8.7177694803256,-72.5435266098529));
#17247=CARTESIAN_POINT('Ctrl Pts',(-2.18235588682236,-8.71775758224027,
-72.5483257588687));
#17248=CARTESIAN_POINT('Ctrl Pts',(-2.18720072261472,-8.7177456909727,-72.5531386962157));
#17249=CARTESIAN_POINT('Ctrl Pts',(-2.19202717238361,-8.71773380791812,
-72.5579651290338));
#17250=CARTESIAN_POINT('Ctrl Pts',(-2.24727143395521,-8.71759779270889,
-72.6132091965836));
#17251=CARTESIAN_POINT('Ctrl Pts',(-2.30034622323894,-8.71746227622743,
-72.670454482637));
#17252=CARTESIAN_POINT('Ctrl Pts',(-2.35125589236409,-8.71732840283244,
-72.7297040492485));
#17253=CARTESIAN_POINT('Ctrl Pts',(-2.40182647150608,-8.71719542111733,
-72.788558976985));
#17254=CARTESIAN_POINT('Ctrl Pts',(-2.45026113238754,-8.71706406067362,
-72.8493921916015));
#17255=CARTESIAN_POINT('Ctrl Pts',(-2.49652311457611,-8.71693544314557,
-72.912237137608));
#17256=CARTESIAN_POINT('Ctrl Pts',(-2.52413192723861,-8.71685868514538,
-72.9497425418081));
#17257=CARTESIAN_POINT('Ctrl Pts',(-2.55096609695345,-8.71678290406618,
-72.9879649889125));
#17258=CARTESIAN_POINT('Ctrl Pts',(-2.57700978828989,-8.7167083383186,-73.0269153964306));
#17259=CARTESIAN_POINT('Ctrl Pts',(-2.63792412174072,-8.71653393436203,
-73.1180176169627));
#17260=CARTESIAN_POINT('Ctrl Pts',(-2.69367621163527,-8.71636874430105,
-73.2118473144967));
#17261=CARTESIAN_POINT('Ctrl Pts',(-2.74421580489452,-8.71621544490872,
-73.3080292596009));
#17262=CARTESIAN_POINT('Ctrl Pts',(-2.78794079145064,-8.71608281594524,
-73.3912423205975));
#17263=CARTESIAN_POINT('Ctrl Pts',(-2.82776422424687,-8.71595908723085,
-73.4762174781629));
#17264=CARTESIAN_POINT('Ctrl Pts',(-2.86363533708147,-8.71584599219185,
-73.5627373263602));
#17265=CARTESIAN_POINT('Ctrl Pts',(-2.89131369256179,-8.715758727414,-73.6294965352409));
#17266=CARTESIAN_POINT('Ctrl Pts',(-2.91676714010597,-8.71567746862,-73.6974992504068));
#17267=CARTESIAN_POINT('Ctrl Pts',(-2.93983939673707,-8.71560303834219,
-73.7664633604219));
#17268=CARTESIAN_POINT('Ctrl Pts',(-2.96289040591261,-8.71552867660791,
-73.8353639607471));
#17269=CARTESIAN_POINT('Ctrl Pts',(-2.98356439031223,-8.71546113081872,
-73.9052237124384));
#17270=CARTESIAN_POINT('Ctrl Pts',(-3.00175318757531,-8.71540122123661,
-73.9757404822145));
#17271=CARTESIAN_POINT('Ctrl Pts',(-3.01622482082387,-8.7153535551107,-74.0318460517753));
#17272=CARTESIAN_POINT('Ctrl Pts',(-3.02912415352737,-8.71531072296457,
-74.0883670360562));
#17273=CARTESIAN_POINT('Ctrl Pts',(-3.04041944202858,-8.71527313793444,
-74.1451449623797));
#17274=CARTESIAN_POINT('Ctrl Pts',(-3.05576944744673,-8.71522206084897,
-74.2223046981938));
#17275=CARTESIAN_POINT('Ctrl Pts',(-3.06811378251743,-8.715180647215,-74.2996825691113));
#17276=CARTESIAN_POINT('Ctrl Pts',(-3.07751063014557,-8.71514903579499,
-74.3772691033185));
#17277=CARTESIAN_POINT('Ctrl Pts',(-3.0869477281149,-8.715117288971,-74.455187970729));
#17278=CARTESIAN_POINT('Ctrl Pts',(-3.09341216521581,-8.71509542851419,
-74.5333180690773));
#17279=CARTESIAN_POINT('Ctrl Pts',(-3.09691174535638,-8.71508359497775,
-74.611661135346));
#17280=CARTESIAN_POINT('Ctrl Pts',(-3.0989402844013,-8.71507673564328,-74.6570728597364));
#17281=CARTESIAN_POINT('Ctrl Pts',(-3.0999716790725,-8.71507324531976,-74.7025562905255));
#17282=CARTESIAN_POINT('Ctrl Pts',(-3.09999942502794,-8.71507315138149,
-74.7481119251981));
#17283=CARTESIAN_POINT('Ctrl Pts',(-3.10003763936464,-8.71507302200089,
-74.810855425439));
#17284=CARTESIAN_POINT('Ctrl Pts',(-3.09816683500873,-8.71507954824019,
-74.8738970593066));
#17285=CARTESIAN_POINT('Ctrl Pts',(-3.09435865722023,-8.71509252803483,
-74.9369344818011));
#17286=CARTESIAN_POINT('Ctrl Pts',(-3.09055434489376,-8.71510549465442,
-74.9999079186372));
#17287=CARTESIAN_POINT('Ctrl Pts',(-3.08481658471838,-8.71512490173472,
-75.0628766666462));
#17288=CARTESIAN_POINT('Ctrl Pts',(-3.07716911332992,-8.71515054782583,
-75.1255399419082));
#17289=CARTESIAN_POINT('Ctrl Pts',(-3.06951203300335,-8.71517622614088,
-75.1882819526766));
#17290=CARTESIAN_POINT('Ctrl Pts',(-3.05994051554409,-8.71520815915505,
-75.2507172406093));
#17291=CARTESIAN_POINT('Ctrl Pts',(-3.04853004779056,-8.71524614465811,
-75.3125518178072));
#17292=CARTESIAN_POINT('Ctrl Pts',(-3.04594441182365,-8.71525475225292,
-75.3265636629177));
#17293=CARTESIAN_POINT('Ctrl Pts',(-3.0432645546154,-8.71526367063402,-75.3405447112827));
#17294=CARTESIAN_POINT('Ctrl Pts',(-3.04049171352755,-8.71527289744857,
-75.3544916376348));
#17295=CARTESIAN_POINT('Ctrl Pts',(-3.02517464325816,-8.71532386602642,
-75.4315339362046));
#17296=CARTESIAN_POINT('Ctrl Pts',(-3.00697437584422,-8.71538409459489,
-75.5077898636854));
#17297=CARTESIAN_POINT('Ctrl Pts',(-2.98591140298778,-8.71545305551348,
-75.5832665200928));
#17298=CARTESIAN_POINT('Ctrl Pts',(-2.9649086222243,-8.71552181936102,-75.6585274852989));
#17299=CARTESIAN_POINT('Ctrl Pts',(-2.94105924077799,-8.71559926572075,
-75.733014372415));
#17300=CARTESIAN_POINT('Ctrl Pts',(-2.91433412241562,-8.71568487146281,
-75.806719746633));
#17301=CARTESIAN_POINT('Ctrl Pts',(-2.8988064503099,-8.71573460961083,-75.8495436124721));
#17302=CARTESIAN_POINT('Ctrl Pts',(-2.8823070876191,-8.71578710218233,-75.8921033293857));
#17303=CARTESIAN_POINT('Ctrl Pts',(-2.86482313746517,-8.71584224657204,
-75.9343936807685));
#17304=CARTESIAN_POINT('Ctrl Pts',(-2.83675354100562,-8.71593077809681,
-76.0022886980269));
#17305=CARTESIAN_POINT('Ctrl Pts',(-2.80623364659306,-8.71602596365631,
-76.0692631955475));
#17306=CARTESIAN_POINT('Ctrl Pts',(-2.77339398152871,-8.71612656968704,
-76.1350219576672));
#17307=CARTESIAN_POINT('Ctrl Pts',(-2.74051886555452,-8.71622728432349,
-76.2008517073547));
#17308=CARTESIAN_POINT('Ctrl Pts',(-2.7053192132796,-8.71633343114044,-76.2654626307996));
#17309=CARTESIAN_POINT('Ctrl Pts',(-2.6679720312962,-8.71644377257514,-76.3285833016415));
#17310=CARTESIAN_POINT('Ctrl Pts',(-2.63928378184157,-8.71652853138252,
-76.3770694645777));
#17311=CARTESIAN_POINT('Ctrl Pts',(-2.60932935209317,-8.71661576524465,
-76.4246767513742));
#17312=CARTESIAN_POINT('Ctrl Pts',(-2.5782058164628,-8.71670491323516,-76.4712945035517));
#17313=CARTESIAN_POINT('Ctrl Pts',(-2.52214838765517,-8.71686548005477,
-76.5552589783755));
#17314=CARTESIAN_POINT('Ctrl Pts',(-2.46186510330967,-8.71703357655273,
-76.6366627857791));
#17315=CARTESIAN_POINT('Ctrl Pts',(-2.39760626728135,-8.7172058063275,-76.7150659498076));
#17316=CARTESIAN_POINT('Ctrl Pts',(-2.33454281768458,-8.71737483216724,
-76.7920106050261));
#17317=CARTESIAN_POINT('Ctrl Pts',(-2.26765065393195,-8.71754783893412,
-76.8660649139989));
#17318=CARTESIAN_POINT('Ctrl Pts',(-2.1972126796686,-8.71772161626889,-76.9368370859082));
#17319=CARTESIAN_POINT('Ctrl Pts',(-2.12477194629744,-8.7179003346052,-77.009621519149));
#17320=CARTESIAN_POINT('Ctrl Pts',(-2.04858089905465,-8.71807986795139,
-77.0789339827324));
#17321=CARTESIAN_POINT('Ctrl Pts',(-1.96899494562744,-8.71825672424842,
-77.1443806932261));
#17322=CARTESIAN_POINT('Ctrl Pts',(-1.88940899220023,-8.71843358054545,
-77.2098274037197));
#17323=CARTESIAN_POINT('Ctrl Pts',(-1.80642841226459,-8.71860775979332,
-77.2714079844154));
#17324=CARTESIAN_POINT('Ctrl Pts',(-1.72045318260168,-8.718775769933,-77.3287673114253));
#17325=CARTESIAN_POINT('',(-1.72045318260168,8.718775769933,-77.3287673114253));
#17326=CARTESIAN_POINT('',(-3.7964050773568E-16,8.72047385811859,-77.85));
#17327=CARTESIAN_POINT('Ctrl Pts',(-1.72045318260166,8.71877576993301,-77.3287673114254));
#17328=CARTESIAN_POINT('Ctrl Pts',(-1.78551125050533,8.71864863546511,-77.2853631006294));
#17329=CARTESIAN_POINT('Ctrl Pts',(-1.84851550918092,8.71851861461283,-77.2397764701245));
#17330=CARTESIAN_POINT('Ctrl Pts',(-1.90951766312105,8.71838686972407,-77.1920774545925));
#17331=CARTESIAN_POINT('Ctrl Pts',(-1.97110904819074,8.71825385228698,-77.1439177054144));
#17332=CARTESIAN_POINT('Ctrl Pts',(-2.03066012128449,8.71811907734696,-77.0936041566429));
#17333=CARTESIAN_POINT('Ctrl Pts',(-2.08819950349703,8.71798374126032,-77.0411618959809));
#17334=CARTESIAN_POINT('Ctrl Pts',(-2.12290656241685,8.7179021081709,-77.0095293590872));
#17335=CARTESIAN_POINT('Ctrl Pts',(-2.15688117527828,8.71782027091635,-76.9771214408884));
#17336=CARTESIAN_POINT('Ctrl Pts',(-2.19012387534448,8.71773849205049,-76.9439365101675));
#17337=CARTESIAN_POINT('Ctrl Pts',(-2.23807228578435,8.71762053633037,-76.8960714247366));
#17338=CARTESIAN_POINT('Ctrl Pts',(-2.28466721546423,8.7175022835572,-76.8464130966564));
#17339=CARTESIAN_POINT('Ctrl Pts',(-2.3296650707744,8.7173849984541,-76.795155411702));
#17340=CARTESIAN_POINT('Ctrl Pts',(-2.37462503718522,8.71726781210689,-76.7439408865215));
#17341=CARTESIAN_POINT('Ctrl Pts',(-2.41799024538773,8.71715159180084,-76.6911300427942));
#17342=CARTESIAN_POINT('Ctrl Pts',(-2.45955419545791,8.71703759906697,-76.6369534068454));
#17343=CARTESIAN_POINT('Ctrl Pts',(-2.50040182112492,8.71692557091482,-76.5837104657535));
#17344=CARTESIAN_POINT('Ctrl Pts',(-2.53950956633579,8.71681569421533,-76.5291488734177));
#17345=CARTESIAN_POINT('Ctrl Pts',(-2.57672055083978,8.71670916639245,-76.4735171025783));
#17346=CARTESIAN_POINT('Ctrl Pts',(-2.62048380112934,8.71658388070496,-76.4080894568509));
#17347=CARTESIAN_POINT('Ctrl Pts',(-2.66157063421398,8.71646333904376,-76.3412785006447));
#17348=CARTESIAN_POINT('Ctrl Pts',(-2.70002458033065,8.71634842363173,-76.2731110483515));
#17349=CARTESIAN_POINT('Ctrl Pts',(-2.73858537466607,8.71623318891549,-76.2047541858263));
#17350=CARTESIAN_POINT('Ctrl Pts',(-2.77449903809121,8.71612361175808,-76.1350326040181));
#17351=CARTESIAN_POINT('Ctrl Pts',(-2.80776603790274,8.71602058175687,-76.063944396236));
#17352=CARTESIAN_POINT('Ctrl Pts',(-2.8269613262682,8.71596113273548,-76.0229260099826));
#17353=CARTESIAN_POINT('Ctrl Pts',(-2.84527460480386,8.71590386350438,-75.9814521402428));
#17354=CARTESIAN_POINT('Ctrl Pts',(-2.86269864862687,8.71584894496138,-75.9395194185678));
#17355=CARTESIAN_POINT('Ctrl Pts',(-2.88692761794546,8.71577257809116,-75.8812099562394));
#17356=CARTESIAN_POINT('Ctrl Pts',(-2.9094770889549,8.71570078483281,-75.8219033957506));
#17357=CARTESIAN_POINT('Ctrl Pts',(-2.93020813456406,8.71563414597153,-75.7618696991879));
#17358=CARTESIAN_POINT('Ctrl Pts',(-2.95092195111498,8.71556756249215,-75.7018858951427));
#17359=CARTESIAN_POINT('Ctrl Pts',(-2.96982017704862,8.71550612484602,-75.6411766139907));
#17360=CARTESIAN_POINT('Ctrl Pts',(-2.98681268740842,8.71545041237147,-75.5800301020663));
#17361=CARTESIAN_POINT('Ctrl Pts',(-3.00382970566113,8.71539461954415,-75.5187953999844));
#17362=CARTESIAN_POINT('Ctrl Pts',(-3.01893539773509,8.7153445684149,-75.4571226823428));
#17363=CARTESIAN_POINT('Ctrl Pts',(-3.03209012160052,8.71530084083237,-75.3953134854414));
#17364=CARTESIAN_POINT('Ctrl Pts',(-3.03483210777939,8.71529172620342,-75.3824299034397));
#17365=CARTESIAN_POINT('Ctrl Pts',(-3.03748950746607,8.7152828863182,-75.3695404189203));
#17366=CARTESIAN_POINT('Ctrl Pts',(-3.04006224424406,8.71527432644609,-75.3566477982502));
#17367=CARTESIAN_POINT('Ctrl Pts',(-3.05540807035026,8.71522326863485,-75.2797460659984));
#17368=CARTESIAN_POINT('Ctrl Pts',(-3.06780605637265,8.71518167516255,-75.2024339736059));
#17369=CARTESIAN_POINT('Ctrl Pts',(-3.07727021873385,8.71514983838311,-75.1247105561547));
#17370=CARTESIAN_POINT('Ctrl Pts',(-3.08669333243792,8.71511813968849,-75.0473242463938));
#17371=CARTESIAN_POINT('Ctrl Pts',(-3.09320807389713,8.7150961132354,-74.9695293973752));
#17372=CARTESIAN_POINT('Ctrl Pts',(-3.09677711036136,8.7150840475902,-74.8913206592895));
#17373=CARTESIAN_POINT('Ctrl Pts',(-3.09886784950679,8.71507697954342,-74.8455060334458));
#17374=CARTESIAN_POINT('Ctrl Pts',(-3.09994676922755,8.7150733296559,-74.7995493518158));
#17375=CARTESIAN_POINT('Ctrl Pts',(-3.09999807972757,8.71507315593626,-74.7534504616245));
#17376=CARTESIAN_POINT('Ctrl Pts',(-3.10009072223195,8.71507284228071,-74.6702176606448));
#17377=CARTESIAN_POINT('Ctrl Pts',(-3.09682687049161,8.71508405787463,-74.5870270480835));
#17378=CARTESIAN_POINT('Ctrl Pts',(-3.09024312842374,8.71510632342949,-74.5042411604237));
#17379=CARTESIAN_POINT('Ctrl Pts',(-3.08365223666089,8.71512861316389,-74.4213653704198));
#17380=CARTESIAN_POINT('Ctrl Pts',(-3.07373433760075,8.71516197687195,-74.3388957004902));
#17381=CARTESIAN_POINT('Ctrl Pts',(-3.06057750882953,8.71520593370195,-74.257186330905));
#17382=CARTESIAN_POINT('Ctrl Pts',(-3.05469194827621,8.7152255972994,-74.2206345560944));
#17383=CARTESIAN_POINT('Ctrl Pts',(-3.04815891436369,8.71524738070808,-74.1842347523213));
#17384=CARTESIAN_POINT('Ctrl Pts',(-3.04098950787876,8.71527124088319,-74.1480175974571));
#17385=CARTESIAN_POINT('Ctrl Pts',(-3.02305629236416,8.71533092360076,-74.0574257130564));
#17386=CARTESIAN_POINT('Ctrl Pts',(-3.0010173356265,8.71540396717694,-73.9673660698357));
#17387=CARTESIAN_POINT('Ctrl Pts',(-2.97490774237264,8.71548918236498,-73.8782638447493));
#17388=CARTESIAN_POINT('Ctrl Pts',(-2.94884511938841,8.71557424425379,-73.7893219115332));
#17389=CARTESIAN_POINT('Ctrl Pts',(-2.9187265192217,8.71567143400121,-73.7013344257932));
#17390=CARTESIAN_POINT('Ctrl Pts',(-2.88463864710567,8.71577956876717,-73.6147203535585));
#17391=CARTESIAN_POINT('Ctrl Pts',(-2.87821859643875,8.71579993468129,-73.5984076095326));
#17392=CARTESIAN_POINT('Ctrl Pts',(-2.87165789742049,8.71582068882947,-73.5821435593562));
#17393=CARTESIAN_POINT('Ctrl Pts',(-2.86495733316071,8.71584182330963,-73.5659309652015));
#17394=CARTESIAN_POINT('Ctrl Pts',(-2.83496309072156,8.71593642918116,-73.4933573041199));
#17395=CARTESIAN_POINT('Ctrl Pts',(-2.80237842122547,8.71603785674922,-73.4223165330266));
#17396=CARTESIAN_POINT('Ctrl Pts',(-2.76726820343563,8.71614516205026,-73.3527789400907));
#17397=CARTESIAN_POINT('Ctrl Pts',(-2.73192387853955,8.71625318283913,-73.2827776859848));
#17398=CARTESIAN_POINT('Ctrl Pts',(-2.69401991232817,8.71636716000513,-73.2142989993937));
#17399=CARTESIAN_POINT('Ctrl Pts',(-2.65357271943122,8.71648613057612,-73.1473297835517));
#17400=CARTESIAN_POINT('Ctrl Pts',(-2.62982116648544,8.71655599292289,-73.1080038684045));
#17401=CARTESIAN_POINT('Ctrl Pts',(-2.60519171261152,8.71662757715425,-73.0691988464413));
#17402=CARTESIAN_POINT('Ctrl Pts',(-2.57968045483705,8.7167006882747,-73.0309163048497));
#17403=CARTESIAN_POINT('Ctrl Pts',(-2.5444843609743,8.71680155456206,-72.9781005660462));
#17404=CARTESIAN_POINT('Ctrl Pts',(-2.50748856662359,8.7169057382801,-72.9261068538568));
#17405=CARTESIAN_POINT('Ctrl Pts',(-2.46883456203953,8.71701213292141,-72.8752051031435));
#17406=CARTESIAN_POINT('Ctrl Pts',(-2.43022702536167,8.71711839966041,-72.8243645439627));
#17407=CARTESIAN_POINT('Ctrl Pts',(-2.38996552511782,8.71722687201015,-72.7746137358733));
#17408=CARTESIAN_POINT('Ctrl Pts',(-2.34823420078443,8.71733644744896,-72.72619266276));
#17409=CARTESIAN_POINT('Ctrl Pts',(-2.30646796846453,8.71744611454693,-72.6777310857281));
#17410=CARTESIAN_POINT('Ctrl Pts',(-2.2632297813738,8.7175568865802,-72.6306018338344));
#17411=CARTESIAN_POINT('Ctrl Pts',(-2.21874306936807,8.71766765825803,-72.5850105792103));
#17412=CARTESIAN_POINT('Ctrl Pts',(-2.21042548426694,8.71768836900098,-72.5764864801456));
#17413=CARTESIAN_POINT('Ctrl Pts',(-2.20206435511428,8.71770907973151,-72.5680160381373));
#17414=CARTESIAN_POINT('Ctrl Pts',(-2.19366127714957,8.71772978322563,-72.5596004471479));
#17415=CARTESIAN_POINT('Ctrl Pts',(-2.13806407215614,8.71786676355723,-72.5039204523483));
#17416=CARTESIAN_POINT('Ctrl Pts',(-2.08053732388198,8.71800360659784,-72.4505417303145));
#17417=CARTESIAN_POINT('Ctrl Pts',(-2.02110377686798,8.71813911894957,-72.3994384664234));
#17418=CARTESIAN_POINT('Ctrl Pts',(-1.96169567378192,8.71827457328749,-72.3483570802063));
#17419=CARTESIAN_POINT('Ctrl Pts',(-1.90038180568892,8.71840869807565,-72.2995486945324));
#17420=CARTESIAN_POINT('Ctrl Pts',(-1.83715014326873,8.71854030144823,-72.2530259610705));
#17421=CARTESIAN_POINT('Ctrl Pts',(-1.80069112902299,8.7186161831988,-72.2262012195231));
#17422=CARTESIAN_POINT('Ctrl Pts',(-1.76359392599721,8.71869122667714,-72.2001371210064));
#17423=CARTESIAN_POINT('Ctrl Pts',(-1.72585219029124,8.71876520340843,-72.1748428752274));
#17424=CARTESIAN_POINT('Ctrl Pts',(-1.67057600678017,8.71887354901836,-72.1377971658741));
#17425=CARTESIAN_POINT('Ctrl Pts',(-1.61393953676665,8.7189794375954,-72.1024241924786));
#17426=CARTESIAN_POINT('Ctrl Pts',(-1.55619057584157,8.71908179680457,-72.0689049081277));
#17427=CARTESIAN_POINT('Ctrl Pts',(-1.49695085761279,8.71918679835978,-72.0345203420962));
#17428=CARTESIAN_POINT('Ctrl Pts',(-1.4365408171687,8.71928808597786,-72.002086896522));
#17429=CARTESIAN_POINT('Ctrl Pts',(-1.37525723990444,8.71938450211639,-71.9717509967445));
#17430=CARTESIAN_POINT('Ctrl Pts',(-1.31397366264018,8.71948091825493,-71.9414150969669));
#17431=CARTESIAN_POINT('Ctrl Pts',(-1.25181708431349,8.71957246291391,-71.9131769381707));
#17432=CARTESIAN_POINT('Ctrl Pts',(-1.18910632066891,8.71965797855096,-71.8871297343147));
#17433=CARTESIAN_POINT('Ctrl Pts',(-1.11705587592624,8.71975623025966,-71.8572032509957));
#17434=CARTESIAN_POINT('Ctrl Pts',(-1.04397150370732,8.71984713239851,-71.8300318288547));
#17435=CARTESIAN_POINT('Ctrl Pts',(-0.969846700918411,8.71992982453554,
-71.8056159597095));
#17436=CARTESIAN_POINT('Ctrl Pts',(-0.896267451190071,8.72001190806457,
-71.7813797895535));
#17437=CARTESIAN_POINT('Ctrl Pts',(-0.821662287246619,8.72008590199707,
-71.7598585810759));
#17438=CARTESIAN_POINT('Ctrl Pts',(-0.746012928529198,8.72015096475974,
-71.7411024094418));
#17439=CARTESIAN_POINT('Ctrl Pts',(-0.700547699498278,8.72019006744951,
-71.7298299591058));
#17440=CARTESIAN_POINT('Ctrl Pts',(-0.654705126074108,8.72022594419686,
-71.7195572105806));
#17441=CARTESIAN_POINT('Ctrl Pts',(-0.608480864241395,8.72025841231196,
-71.7103041208285));
#17442=CARTESIAN_POINT('Ctrl Pts',(-0.522148965568356,8.72031905219915,
-71.6930223563349));
#17443=CARTESIAN_POINT('Ctrl Pts',(-0.435577747650747,8.72036694530415,
-71.6795137228333));
#17444=CARTESIAN_POINT('Ctrl Pts',(-0.348874115493963,8.72040190807551,
-71.6696937081618));
#17445=CARTESIAN_POINT('Ctrl Pts',(-0.260977259244963,8.72043735200805,
-71.6597385494622));
#17446=CARTESIAN_POINT('Ctrl Pts',(-0.172943401919679,8.7204595072609,-71.6535739789158));
#17447=CARTESIAN_POINT('Ctrl Pts',(-0.0848655614443662,8.7204681825997,
-71.651161857005));
#17448=CARTESIAN_POINT('Ctrl Pts',(-0.0579277116901832,8.72047083587744,
-71.6504241302707));
#17449=CARTESIAN_POINT('Ctrl Pts',(-0.0309856732385336,8.72047222825804,
-71.6500377660259));
#17450=CARTESIAN_POINT('Ctrl Pts',(-0.0040419767996967,8.72047235427065,
-71.6500026350941));
#17451=CARTESIAN_POINT('Ctrl Pts',(0.0656511889534763,8.72047268021767,
-71.649911764643));
#17452=CARTESIAN_POINT('Ctrl Pts',(0.135650971586711,8.72046435621686,-71.6521750422896));
#17453=CARTESIAN_POINT('Ctrl Pts',(0.205643835986415,8.72044761722972,-71.656828389384));
#17454=CARTESIAN_POINT('Ctrl Pts',(0.275574141809366,8.72043089320364,-71.6614775773863));
#17455=CARTESIAN_POINT('Ctrl Pts',(0.34549702755091,8.72040576922689,-71.6685125833512));
#17456=CARTESIAN_POINT('Ctrl Pts',(0.415099098091722,8.7203724796315,-71.6779171985828));
#17457=CARTESIAN_POINT('Ctrl Pts',(0.477690824307086,8.72034254297553,-71.686374577755));
#17458=CARTESIAN_POINT('Ctrl Pts',(0.540022838919696,8.7203060027519,-71.6967475564138));
#17459=CARTESIAN_POINT('Ctrl Pts',(0.601871906508907,8.7202630293788,-71.7089886208442));
#17460=CARTESIAN_POINT('Ctrl Pts',(0.679072088375951,8.72020938989241,-71.7242679522408));
#17461=CARTESIAN_POINT('Ctrl Pts',(0.755342636959279,8.72014612775218,-71.7424137714015));
#17462=CARTESIAN_POINT('Ctrl Pts',(0.830696162389788,8.72007401553564,-71.7633724896146));
#17463=CARTESIAN_POINT('Ctrl Pts',(0.90631596771332,8.72000164849316,-71.7844052705237));
#17464=CARTESIAN_POINT('Ctrl Pts',(0.981013023994232,8.71992036871607,-71.8082710473993));
#17465=CARTESIAN_POINT('Ctrl Pts',(1.05479044243209,8.71983095700113,-71.8349670460604));
#17466=CARTESIAN_POINT('Ctrl Pts',(1.09744379364417,8.71977926490672,-71.8504009529517));
#17467=CARTESIAN_POINT('Ctrl Pts',(1.1397895247603,8.71972485478723,-71.8667817755452));
#17468=CARTESIAN_POINT('Ctrl Pts',(1.18182525825237,8.71966787752108,-71.8841163563472));
#17469=CARTESIAN_POINT('Ctrl Pts',(1.23993985422713,8.71958910618709,-71.9080814944812));
#17470=CARTESIAN_POINT('Ctrl Pts',(1.29758981844413,8.71950512323467,-71.9339279864301));
#17471=CARTESIAN_POINT('Ctrl Pts',(1.35448544537096,8.71941691938241,-71.9615651023776));
#17472=CARTESIAN_POINT('Ctrl Pts',(1.41132820424855,8.71932879749014,-71.9891765376097));
#17473=CARTESIAN_POINT('Ctrl Pts',(1.46741757631549,8.71923646253861,-72.0185750874006));
#17474=CARTESIAN_POINT('Ctrl Pts',(1.52248529254967,8.71914090248724,-72.0496225200965));
#17475=CARTESIAN_POINT('Ctrl Pts',(1.57762775617506,8.71904521272529,-72.0807120957167));
#17476=CARTESIAN_POINT('Ctrl Pts',(1.6317453729977,8.71894628910224,-72.1134547768304));
#17477=CARTESIAN_POINT('Ctrl Pts',(1.68459601055329,8.71884512360603,-72.147667146342));
#17478=CARTESIAN_POINT('Ctrl Pts',(1.6963074091596,8.71882270591145,-72.1552484114912));
#17479=CARTESIAN_POINT('Ctrl Pts',(1.70795671337826,8.71880017813187,-72.1629016800187));
#17480=CARTESIAN_POINT('Ctrl Pts',(1.71954149938841,8.7187775510613,-72.1706246818501));
#17481=CARTESIAN_POINT('Ctrl Pts',(1.78484836218897,8.71864999557673,-72.2141615258255));
#17482=CARTESIAN_POINT('Ctrl Pts',(1.84834464661823,8.71851898320049,-72.2600686341301));
#17483=CARTESIAN_POINT('Ctrl Pts',(1.91004281928277,8.71838568792874,-72.3083332683377));
#17484=CARTESIAN_POINT('Ctrl Pts',(1.97151884582345,8.71825287259062,-72.3564241242803));
#17485=CARTESIAN_POINT('Ctrl Pts',(2.03121027972591,8.71811779076666,-72.4068560638889));
#17486=CARTESIAN_POINT('Ctrl Pts',(2.08909679274718,8.71798160381756,-72.4596562287435));
#17487=CARTESIAN_POINT('Ctrl Pts',(2.12285709209413,8.71790217750685,-72.490450092081));
#17488=CARTESIAN_POINT('Ctrl Pts',(2.15600280759306,8.7178223752988,-72.5220501914981));
#17489=CARTESIAN_POINT('Ctrl Pts',(2.18852355201527,8.71774242757821,-72.5544671120035));
#17490=CARTESIAN_POINT('Ctrl Pts',(2.2433386200597,8.71760767236821,-72.6091071805155));
#17491=CARTESIAN_POINT('Ctrl Pts',(2.29612570674144,8.71747318196186,-72.6658244324568));
#17492=CARTESIAN_POINT('Ctrl Pts',(2.34666019741014,8.71734056635167,-72.7243677732888));
#17493=CARTESIAN_POINT('Ctrl Pts',(2.39724915531344,8.71720780780533,-72.782974213478));
#17494=CARTESIAN_POINT('Ctrl Pts',(2.44558033542279,8.7170769280987,-72.8434102611175));
#17495=CARTESIAN_POINT('Ctrl Pts',(2.49146986090751,8.71694954243573,-72.9053922009843));
#17496=CARTESIAN_POINT('Ctrl Pts',(2.52036735992414,8.71686932528309,-72.9444233966097));
#17497=CARTESIAN_POINT('Ctrl Pts',(2.54829748073016,8.71679049367888,-72.9840669932305));
#17498=CARTESIAN_POINT('Ctrl Pts',(2.57522351763586,8.71671345095951,-73.0242468791235));
#17499=CARTESIAN_POINT('Ctrl Pts',(2.63903811929646,8.71653086001733,-73.1194730508029));
#17500=CARTESIAN_POINT('Ctrl Pts',(2.6977347010216,8.71635675547632,-73.2184900268912));
#17501=CARTESIAN_POINT('Ctrl Pts',(2.7508937881556,8.71619515040142,-73.3208102413301));
#17502=CARTESIAN_POINT('Ctrl Pts',(2.79136462501235,8.71607211795346,-73.3987082062682));
#17503=CARTESIAN_POINT('Ctrl Pts',(2.82862636615098,8.71595633021215,-73.4785198992802));
#17504=CARTESIAN_POINT('Ctrl Pts',(2.86250414971471,8.7158495579803,-73.5600126081063));
#17505=CARTESIAN_POINT('Ctrl Pts',(2.89262433742607,8.7157546285213,-73.6324664533329));
#17506=CARTESIAN_POINT('Ctrl Pts',(2.9198272202729,8.71566755898673,-73.7056522605558));
#17507=CARTESIAN_POINT('Ctrl Pts',(2.94418325530203,8.71558882104429,-73.7795439426748));
#17508=CARTESIAN_POINT('Ctrl Pts',(2.96871928819064,8.71550950120659,-73.8539817048351));
#17509=CARTESIAN_POINT('Ctrl Pts',(2.99036654369563,8.71543863656162,-73.9291365337836));
#17510=CARTESIAN_POINT('Ctrl Pts',(3.00914988290531,8.7153767093118,-74.0050053810859));
#17511=CARTESIAN_POINT('Ctrl Pts',(3.02023921888543,8.71534014860916,-74.0497969449696));
#17512=CARTESIAN_POINT('Ctrl Pts',(3.03032941905769,8.71530670303841,-74.0948377738576));
#17513=CARTESIAN_POINT('Ctrl Pts',(3.03941737224908,8.71527647182606,-74.1401294913914));
#17514=CARTESIAN_POINT('Ctrl Pts',(3.05202223556094,8.71523454155954,-74.2029484668691));
#17515=CARTESIAN_POINT('Ctrl Pts',(3.06273741417212,8.71519884659067,-74.2664684112262));
#17516=CARTESIAN_POINT('Ctrl Pts',(3.07147100678526,8.71516962114423,-74.3303979808467));
#17517=CARTESIAN_POINT('Ctrl Pts',(3.08019384996495,8.7151404316689,-74.3942488650183));
#17518=CARTESIAN_POINT('Ctrl Pts',(3.08693987329442,8.71511769580024,-74.4585078864968));
#17519=CARTESIAN_POINT('Ctrl Pts',(3.09166849006865,8.71510164689924,-74.5228745995784));
#17520=CARTESIAN_POINT('Ctrl Pts',(3.09640032601161,8.71508558707239,-74.5872851325169));
#17521=CARTESIAN_POINT('Ctrl Pts',(3.09911198139106,8.71507622332107,-74.6518030104008));
#17522=CARTESIAN_POINT('Ctrl Pts',(3.09981490362319,8.7150737894832,-74.7161242966772));
#17523=CARTESIAN_POINT('Ctrl Pts',(3.09992480125886,8.71507340896738,-74.7261805404008));
#17524=CARTESIAN_POINT('Ctrl Pts',(3.09998570215258,8.71507319784241,-74.7362319816975));
#17525=CARTESIAN_POINT('Ctrl Pts',(3.09999776495605,8.71507315700192,-74.7462774649036));
#17526=CARTESIAN_POINT('Ctrl Pts',(3.10009227788373,8.71507283701379,-74.8249845440814));
#17527=CARTESIAN_POINT('Ctrl Pts',(3.09719331507636,8.71508265594522,-74.9034127826038));
#17528=CARTESIAN_POINT('Ctrl Pts',(3.09133919636591,8.71510242433115,-74.9815641876711));
#17529=CARTESIAN_POINT('Ctrl Pts',(3.08548314057808,8.71512219925826,-75.0597414523644));
#17530=CARTESIAN_POINT('Ctrl Pts',(3.07666991689266,8.71515193022534,-75.1376424855042));
#17531=CARTESIAN_POINT('Ctrl Pts',(3.06488602188168,8.71519142757921,-75.2152673133526));
#17532=CARTESIAN_POINT('Ctrl Pts',(3.05809788687412,8.7152141801046,-75.2599832422439));
#17533=CARTESIAN_POINT('Ctrl Pts',(3.05032302065739,8.71524017346659,-75.3046074173627));
#17534=CARTESIAN_POINT('Ctrl Pts',(3.04155119258465,8.71526937141208,-75.3491379998689));
#17535=CARTESIAN_POINT('Ctrl Pts',(3.02892216945727,8.71531140843399,-75.4132498077707));
#17536=CARTESIAN_POINT('Ctrl Pts',(3.0142188489071,8.71536027865207,-75.4771795507943));
#17537=CARTESIAN_POINT('Ctrl Pts',(2.99748430077214,8.7154153389999,-75.5406249848219));
#17538=CARTESIAN_POINT('Ctrl Pts',(2.98075705308234,8.71547037532765,-75.6040427407844));
#17539=CARTESIAN_POINT('Ctrl Pts',(2.96200046149881,8.71553159638542,-75.6669761251053));
#17540=CARTESIAN_POINT('Ctrl Pts',(2.94130818425555,8.715598359948,-75.7291354172082));
#17541=CARTESIAN_POINT('Ctrl Pts',(2.92058308127345,8.71566522942272,-75.7913933173407));
#17542=CARTESIAN_POINT('Ctrl Pts',(2.89791633652228,8.71573765900119,-75.852874205843));
#17543=CARTESIAN_POINT('Ctrl Pts',(2.87345062347374,8.71581500339693,-75.913306285747));
#17544=CARTESIAN_POINT('Ctrl Pts',(2.87088533059335,8.71582311315557,-75.9196427446116));
#17545=CARTESIAN_POINT('Ctrl Pts',(2.86830030198674,8.71583127694801,-75.9259676939315));
#17546=CARTESIAN_POINT('Ctrl Pts',(2.86569573146446,8.71583949403039,-75.9322808357858));
#17547=CARTESIAN_POINT('Ctrl Pts',(2.83589947953976,8.71593349734293,-76.0045030941273));
#17548=CARTESIAN_POINT('Ctrl Pts',(2.8034223737145,8.71603465697795,-76.0754905992693));
#17549=CARTESIAN_POINT('Ctrl Pts',(2.7682632632438,8.71614215617445,-76.1452485460931));
#17550=CARTESIAN_POINT('Ctrl Pts',(2.73333830122917,8.71624893946059,-76.2145419272516));
#17551=CARTESIAN_POINT('Ctrl Pts',(2.69576654364044,8.71636197815047,-76.2826227303007));
#17552=CARTESIAN_POINT('Ctrl Pts',(2.65550299926957,8.71648047169272,-76.3494698561931));
#17553=CARTESIAN_POINT('Ctrl Pts',(2.63147426775503,8.71655118701492,-76.389363304862));
#17554=CARTESIAN_POINT('Ctrl Pts',(2.60648603157346,8.71662384510397,-76.4288168269235));
#17555=CARTESIAN_POINT('Ctrl Pts',(2.58052213110435,8.7166982758045,-76.4678199937365));
#17556=CARTESIAN_POINT('Ctrl Pts',(2.51978387254882,8.71687239414,-76.5590614631446));
#17557=CARTESIAN_POINT('Ctrl Pts',(2.45454347352631,8.71705377090808,-76.6465825710347));
#17558=CARTESIAN_POINT('Ctrl Pts',(2.38512830596815,8.71723875234124,-76.7301926583213));
#17559=CARTESIAN_POINT('Ctrl Pts',(2.32509433867442,8.71739873422559,-76.8025031550349));
#17560=CARTESIAN_POINT('Ctrl Pts',(2.26193646115044,8.71756141229847,-76.8718888973876));
#17561=CARTESIAN_POINT('Ctrl Pts',(2.19583586053567,8.71772442298748,-76.938219567042));
#17562=CARTESIAN_POINT('Ctrl Pts',(2.14482140248578,8.71785022974081,-76.989411585466));
#17563=CARTESIAN_POINT('Ctrl Pts',(2.09180437250501,8.71797683907039,-77.0390266616564));
#17564=CARTESIAN_POINT('Ctrl Pts',(2.03698524923165,8.71810275138921,-77.086812164983));
#17565=CARTESIAN_POINT('Ctrl Pts',(1.9822166052559,8.71822854776373,-77.1345536658066));
#17566=CARTESIAN_POINT('Ctrl Pts',(1.92564953905691,8.71835364841055,-77.1804685789439));
#17567=CARTESIAN_POINT('Ctrl Pts',(1.8675214937686,8.71847655788148,-77.2243410173847));
#17568=CARTESIAN_POINT('Ctrl Pts',(1.8212762647317,8.7185743416037,-77.2592448396969));
#17569=CARTESIAN_POINT('Ctrl Pts',(1.77404384024149,8.71867073844341,-77.2928565446377));
#17570=CARTESIAN_POINT('Ctrl Pts',(1.72595832697208,8.71876499536582,-77.325085989546));
#17571=CARTESIAN_POINT('Ctrl Pts',(1.66060795844858,8.71889309474955,-77.3688872502346));
#17572=CARTESIAN_POINT('Ctrl Pts',(1.59390205777866,8.71901683731767,-77.4099970252329));
#17573=CARTESIAN_POINT('Ctrl Pts',(1.52587171097307,8.71913520491618,-77.4484654012331));
#17574=CARTESIAN_POINT('Ctrl Pts',(1.45754995827931,8.71925407953864,-77.4870985553332));
#17575=CARTESIAN_POINT('Ctrl Pts',(1.38789172230878,8.71936753304584,-77.5230680523986));
#17576=CARTESIAN_POINT('Ctrl Pts',(1.31689839475672,8.71947453414395,-77.5563817662405));
#17577=CARTESIAN_POINT('Ctrl Pts',(1.27574673754136,8.71953655789551,-77.5756922363912));
#17578=CARTESIAN_POINT('Ctrl Pts',(1.23414598119487,8.71959641363605,-77.5941095315021));
#17579=CARTESIAN_POINT('Ctrl Pts',(1.19209316853417,8.71965390050633,-77.6116278370072));
#17580=CARTESIAN_POINT('Ctrl Pts',(1.13417431668521,8.71973307650698,-77.6357555962935));
#17581=CARTESIAN_POINT('Ctrl Pts',(1.07524714468821,8.71980778376098,-77.6582351681579));
#17582=CARTESIAN_POINT('Ctrl Pts',(1.01557993119606,8.71987734230788,-77.6789242740897));
#17583=CARTESIAN_POINT('Ctrl Pts',(0.955973288844866,8.71994683024247,-77.6995923774864));
#17584=CARTESIAN_POINT('Ctrl Pts',(0.895628553388487,8.72001117991806,-77.7184734566331));
#17585=CARTESIAN_POINT('Ctrl Pts',(0.834832564457375,8.72006971344289,-77.7354739304375));
#17586=CARTESIAN_POINT('Ctrl Pts',(0.773960195248435,8.72012832050558,-77.7524957625738));
#17587=CARTESIAN_POINT('Ctrl Pts',(0.712635912251662,8.72018109679423,-77.7676321462886));
#17588=CARTESIAN_POINT('Ctrl Pts',(0.651160151409611,8.72022736185888,-77.7808398930356));
#17589=CARTESIAN_POINT('Ctrl Pts',(0.637229636273559,8.72023784560361,-77.7838327915936));
#17590=CARTESIAN_POINT('Ctrl Pts',(0.623291377035618,8.7202479950077,-77.786726866896));
#17591=CARTESIAN_POINT('Ctrl Pts',(0.609348919153831,8.72025780215369,-77.7895219845769));
#17592=CARTESIAN_POINT('Ctrl Pts',(0.532331146878382,8.72031197657134,-77.80496214146));
#17593=CARTESIAN_POINT('Ctrl Pts',(0.454932360941475,8.72035618745966,-77.817438170274));
#17594=CARTESIAN_POINT('Ctrl Pts',(0.377153874529794,8.72039009691618,-77.8269717182528));
#17595=CARTESIAN_POINT('Ctrl Pts',(0.299597654310796,8.72042390947025,-77.8364780223816));
#17596=CARTESIAN_POINT('Ctrl Pts',(0.221663122665409,8.72044747938484,-77.8430587096567));
#17597=CARTESIAN_POINT('Ctrl Pts',(0.143345956999472,8.72046047164607,-77.8466840227269));
#17598=CARTESIAN_POINT('Ctrl Pts',(0.0978426785326954,8.7204680203166,-77.8487903761522));
#17599=CARTESIAN_POINT('Ctrl Pts',(0.0522101865630996,8.72047199822613,
-77.849898103416));
#17600=CARTESIAN_POINT('Ctrl Pts',(0.00644834567061791,8.72047233966639,
-77.8499932933537));
#17601=CARTESIAN_POINT('Ctrl Pts',(0.00429897232490631,8.72047235570339,
-77.8499977642996));
#17602=CARTESIAN_POINT('Ctrl Pts',(0.00214952107544824,8.72047236353894,
-77.85));
#17603=CARTESIAN_POINT('Ctrl Pts',(2.44051389952465E-13,8.72047236318302,
-77.85));
#17604=CARTESIAN_POINT('Ctrl Pts',(2.44051389952465E-13,8.72047236318302,
-77.85));
#17605=CARTESIAN_POINT('Ctrl Pts',(-0.0734697129943097,8.72047235101777,
-77.85));
#17606=CARTESIAN_POINT('Ctrl Pts',(-0.147020943399736,8.72046276921705,
-77.8473838153449));
#17607=CARTESIAN_POINT('Ctrl Pts',(-0.220331040979787,8.72044401589269,
-77.8421601239879));
#17608=CARTESIAN_POINT('Ctrl Pts',(-0.293720869844243,8.72042524217241,
-77.8369307513996));
#17609=CARTESIAN_POINT('Ctrl Pts',(-0.36686851812668,8.72039727696793,-77.8290882481745));
#17610=CARTESIAN_POINT('Ctrl Pts',(-0.439455673807259,8.72036051969141,
-77.8186933230218));
#17611=CARTESIAN_POINT('Ctrl Pts',(-0.493101433774696,8.72033335411349,
-77.8110109217155));
#17612=CARTESIAN_POINT('Ctrl Pts',(-0.546441130541466,8.7203013863108,-77.8019354866522));
#17613=CARTESIAN_POINT('Ctrl Pts',(-0.599350660335006,8.7202647775142,-77.7915092940769));
#17614=CARTESIAN_POINT('Ctrl Pts',(-0.698403651448248,8.72019624145237,
-77.77199021));
#17615=CARTESIAN_POINT('Ctrl Pts',(-0.79671492865933,8.72011052590357,-77.7475859612361));
#17616=CARTESIAN_POINT('Ctrl Pts',(-0.893782127518088,8.72001010025117,
-77.7183587230201));
#17617=CARTESIAN_POINT('Ctrl Pts',(-0.989042986979578,8.71991154343618,
-77.6896753792657));
#17618=CARTESIAN_POINT('Ctrl Pts',(-1.08310524287333,8.71979881890891,-77.6563470409888));
#17619=CARTESIAN_POINT('Ctrl Pts',(-1.17549851467908,8.71967426074279,-77.6184844852269));
#17620=CARTESIAN_POINT('Ctrl Pts',(-1.27051973265046,8.7195461597629,-77.5795450030147));
#17621=CARTESIAN_POINT('Ctrl Pts',(-1.36377517836987,8.71940554240117,-77.5358094936397));
#17622=CARTESIAN_POINT('Ctrl Pts',(-1.45476477794649,8.71925494761406,-77.4874549203314));
#17623=CARTESIAN_POINT('Ctrl Pts',(-1.54575437752311,8.71910435282694,-77.439100347023));
#17624=CARTESIAN_POINT('Ctrl Pts',(-1.6344776757099,8.71894378061444,-77.3861268233915));
#17625=CARTESIAN_POINT('Ctrl Pts',(-1.72045318260166,8.71877576993301,-77.3287673114254));
#17626=CARTESIAN_POINT('Origin',(0.,0.,-78.75));
#17627=CARTESIAN_POINT('',(-6.18146853146853,-7.57011565109303E-16,-189.5));
#17628=CARTESIAN_POINT('',(-8.35,-1.02258007728804E-15,-78.75));
#17629=CARTESIAN_POINT('Origin',(0.,0.,-189.5));
#17630=CARTESIAN_POINT('Origin',(0.,0.,-63.85));
#17631=CARTESIAN_POINT('Origin',(-10.7,-1.31037207508767E-15,-63.85));
#17632=CARTESIAN_POINT('Origin',(0.,-11.5419797204109,-74.75));
#17633=CARTESIAN_POINT('',(-3.7964050773568E-16,-11.5419797204109,-77.85));
#17634=CARTESIAN_POINT('Origin',(-6.18146853146853,0.,-189.5));
#17635=CARTESIAN_POINT('',(3.74438030913772,-3.85,-189.5));
#17636=CARTESIAN_POINT('',(-3.74438030913772,-3.85,-189.5));
#17637=CARTESIAN_POINT('',(-3.55,-3.85,-189.5));
#17638=CARTESIAN_POINT('',(3.74438030913772,3.85,-189.5));
#17639=CARTESIAN_POINT('',(3.74438030913772,-3.85,-189.5));
#17640=CARTESIAN_POINT('',(-3.74438030913772,3.85,-189.5));
#17641=CARTESIAN_POINT('',(-3.55,3.85,-189.5));
#17642=CARTESIAN_POINT('',(-3.74438030913772,-3.85,-189.5));
#17643=CARTESIAN_POINT('Origin',(3.55,-3.85,-188.5));
#17644=CARTESIAN_POINT('',(3.55,-3.85,-188.5));
#17645=CARTESIAN_POINT('',(3.55,-3.85,-188.5));
#17646=CARTESIAN_POINT('',(3.55,3.85,-188.5));
#17647=CARTESIAN_POINT('',(3.55,-3.85,-188.5));
#17648=CARTESIAN_POINT('',(3.29150268371209,3.85,-187.170146593374));
#17649=CARTESIAN_POINT('Origin',(-3.55,3.85,-188.5));
#17650=CARTESIAN_POINT('',(-3.55,3.85,-188.5));
#17651=CARTESIAN_POINT('',(-3.55,3.85,-188.5));
#17652=CARTESIAN_POINT('',(-3.55,3.85,-188.5));
#17653=CARTESIAN_POINT('Origin',(-3.55,-3.85,-188.5));
#17654=CARTESIAN_POINT('',(-3.55,-3.85,-188.5));
#17655=CARTESIAN_POINT('',(-3.55,-3.85,-188.5));
#17656=CARTESIAN_POINT('',(-3.55,-3.85,-188.5));
#17657=CARTESIAN_POINT('Origin',(-3.55,-3.85,-188.5));
#17658=CARTESIAN_POINT('',(-3.55,-3.85,-188.5));
#17659=CARTESIAN_POINT('Origin',(0.,0.,-188.5));
#17660=CARTESIAN_POINT('',(0.,0.,0.));
#17661=CARTESIAN_POINT('',(0.,0.,0.));
#17662=CARTESIAN_POINT('Origin',(-5.60010460205265,-15.5,6.34999999999999));
#17663=CARTESIAN_POINT('',(5.60010460205265,-14.390352550159,6.34999999999999));
#17664=CARTESIAN_POINT('',(-5.60010460205265,-14.390352550159,6.34999999999999));
#17665=CARTESIAN_POINT('Ctrl Pts',(5.6001046019848,-14.3903525501799,6.35));
#17666=CARTESIAN_POINT('Ctrl Pts',(-2.66453525910038E-15,-16.1176005778891,
6.35));
#17667=CARTESIAN_POINT('Ctrl Pts',(-5.60010460198481,-14.3903525501799,
6.35));
#17668=CARTESIAN_POINT('',(5.60010460205265,0.,6.34999999999999));
#17669=CARTESIAN_POINT('',(5.60010460205265,-15.5,6.34999999999999));
#17670=CARTESIAN_POINT('',(-5.60010460205265,0.,6.34999999999999));
#17671=CARTESIAN_POINT('',(-5.60010460205265,0.,6.34999999999999));
#17672=CARTESIAN_POINT('',(-5.60010460205265,-15.5,6.34999999999999));
#17673=CARTESIAN_POINT('Origin',(-6.35,-15.5,5.60010460205265));
#17674=CARTESIAN_POINT('',(-6.35,-14.390352550159,5.60010460205265));
#17675=CARTESIAN_POINT('Ctrl Pts',(-5.60010460206764,-14.3903525501596,
6.349999999985));
#17676=CARTESIAN_POINT('Ctrl Pts',(-5.97505230102632,-14.4058383559469,
5.97505230102632));
#17677=CARTESIAN_POINT('Ctrl Pts',(-6.34999999998501,-14.3903525501596,
5.60010460206763));
#17678=CARTESIAN_POINT('',(-6.35,0.,5.60010460205265));
#17679=CARTESIAN_POINT('',(-6.35,0.,5.60010460205265));
#17680=CARTESIAN_POINT('',(-6.35,-15.5,5.60010460205265));
#17681=CARTESIAN_POINT('Origin',(-6.35,-15.5,5.60010460205265));
#17682=CARTESIAN_POINT('',(-6.35,-14.390352550159,-5.60010460205265));
#17683=CARTESIAN_POINT('Ctrl Pts',(-6.35,-14.3903525501799,5.60010460198479));
#17684=CARTESIAN_POINT('Ctrl Pts',(-6.35,-16.1176005778891,-1.46549439250521E-14));
#17685=CARTESIAN_POINT('Ctrl Pts',(-6.35,-14.3903525501799,-5.60010460198484));
#17686=CARTESIAN_POINT('',(-6.35,0.,-5.60010460205265));
#17687=CARTESIAN_POINT('',(-6.35,0.,5.60010460205265));
#17688=CARTESIAN_POINT('',(-6.35,-15.5,-5.60010460205265));
#17689=CARTESIAN_POINT('Origin',(-6.35,-15.5,-5.60010460205265));
#17690=CARTESIAN_POINT('',(-5.60010460205266,-14.390352550159,-6.34999999999999));
#17691=CARTESIAN_POINT('Ctrl Pts',(-6.34999999998502,-14.3903525501596,
-5.60010460206762));
#17692=CARTESIAN_POINT('Ctrl Pts',(-5.97505230102633,-14.4058383559469,
-5.97505230102631));
#17693=CARTESIAN_POINT('Ctrl Pts',(-5.60010460206764,-14.3903525501596,
-6.349999999985));
#17694=CARTESIAN_POINT('',(-5.60010460205265,0.,-6.34999999999999));
#17695=CARTESIAN_POINT('',(-6.35,0.,-5.60010460205265));
#17696=CARTESIAN_POINT('',(-5.60010460205265,-15.5,-6.34999999999999));
#17697=CARTESIAN_POINT('Origin',(-5.60010460205265,-15.5,-6.34999999999999));
#17698=CARTESIAN_POINT('',(-2.74757696753127E-15,-15.3773491427837,-6.35));
#17699=CARTESIAN_POINT('Ctrl Pts',(-5.60010460198478,-14.3903525501799,
-6.35));
#17700=CARTESIAN_POINT('Ctrl Pts',(-2.40005222287474,-15.3773491427837,
-6.35));
#17701=CARTESIAN_POINT('Ctrl Pts',(-4.71750321760398E-15,-15.3773491427837,
-6.35));
#17702=CARTESIAN_POINT('',(5.60010460205265,0.,-6.34999999999999));
#17703=CARTESIAN_POINT('',(-5.60010460205265,0.,-6.34999999999999));
#17704=CARTESIAN_POINT('',(5.60010460205265,-14.390352550159,-6.34999999999999));
#17705=CARTESIAN_POINT('',(5.60010460205265,-15.5,-6.34999999999999));
#17706=CARTESIAN_POINT('Ctrl Pts',(-4.71750321760398E-15,-15.3773491427837,
-6.35));
#17707=CARTESIAN_POINT('Ctrl Pts',(2.40005222287474,-15.3773491427837,-6.35));
#17708=CARTESIAN_POINT('Ctrl Pts',(5.6001046019848,-14.3903525501799,-6.35));
#17709=CARTESIAN_POINT('Origin',(6.35,-15.5,-5.60010460205265));
#17710=CARTESIAN_POINT('',(6.35,-14.390352550159,-5.60010460205265));
#17711=CARTESIAN_POINT('Ctrl Pts',(5.60010460206764,-14.3903525501596,-6.34999999998499));
#17712=CARTESIAN_POINT('Ctrl Pts',(5.97505230102632,-14.4058383559469,-5.97505230102632));
#17713=CARTESIAN_POINT('Ctrl Pts',(6.349999999985,-14.3903525501596,-5.60010460206764));
#17714=CARTESIAN_POINT('',(6.35,0.,-5.60010460205265));
#17715=CARTESIAN_POINT('',(6.35,0.,-5.60010460205265));
#17716=CARTESIAN_POINT('',(6.35,-15.5,-5.60010460205265));
#17717=CARTESIAN_POINT('Origin',(6.35,-15.5,5.60010460205265));
#17718=CARTESIAN_POINT('',(6.35,-14.390352550159,5.60010460205265));
#17719=CARTESIAN_POINT('Ctrl Pts',(6.35,-14.3903525501799,-5.60010460198479));
#17720=CARTESIAN_POINT('Ctrl Pts',(6.35,-16.1176005778891,1.55431223447522E-15));
#17721=CARTESIAN_POINT('Ctrl Pts',(6.35,-14.3903525501799,5.60010460198479));
#17722=CARTESIAN_POINT('',(6.35,0.,5.60010460205265));
#17723=CARTESIAN_POINT('',(6.35,0.,5.60010460205265));
#17724=CARTESIAN_POINT('',(6.35,-15.5,5.60010460205265));
#17725=CARTESIAN_POINT('',(6.35,-7.99999999999999,2.8));
#17726=CARTESIAN_POINT('Origin',(6.35,-7.99999999999999,0.));
#17727=CARTESIAN_POINT('Origin',(5.60010460205265,-15.5,6.34999999999999));
#17728=CARTESIAN_POINT('Ctrl Pts',(6.34999999998501,-14.3903525501596,5.60010460206765));
#17729=CARTESIAN_POINT('Ctrl Pts',(5.97505230102634,-14.4058383559469,5.97505230102632));
#17730=CARTESIAN_POINT('Ctrl Pts',(5.60010460206767,-14.3903525501596,6.34999999998498));
#17731=CARTESIAN_POINT('',(5.60010460205265,0.,6.34999999999999));
#17732=CARTESIAN_POINT('Origin',(0.,0.,0.));
#17733=CARTESIAN_POINT('',(0.,2.99999999999999,17.85));
#17734=CARTESIAN_POINT('Origin',(0.,2.99999999999999,0.));
#17735=CARTESIAN_POINT('',(0.,9.79999999999999,17.85));
#17736=CARTESIAN_POINT('',(-2.18599453647803E-15,0.,17.85));
#17737=CARTESIAN_POINT('',(-6.98315068203329E-17,18.1,17.85));
#17738=CARTESIAN_POINT('',(8.24516586553328E-17,0.,17.85));
#17739=CARTESIAN_POINT('',(-2.18599453647803E-15,19.5,17.85));
#17740=CARTESIAN_POINT('',(-2.18599453647803E-15,0.,17.85));
#17741=CARTESIAN_POINT('Origin',(0.,19.5,0.));
#17742=CARTESIAN_POINT('',(-6.98315068203329E-17,18.1,-17.85));
#17743=CARTESIAN_POINT('Origin',(0.,18.1,0.));
#17744=CARTESIAN_POINT('',(0.,9.79999999999999,-17.85));
#17745=CARTESIAN_POINT('',(8.24516586553328E-17,0.,-17.85));
#17746=CARTESIAN_POINT('Origin',(0.,9.79999999999999,0.));
#17747=CARTESIAN_POINT('Origin',(0.,24.,0.));
#17748=CARTESIAN_POINT('',(-2.44929359829471E-15,24.,20.));
#17749=CARTESIAN_POINT('Origin',(0.,24.,0.));
#17750=CARTESIAN_POINT('',(-1.83697019872103E-15,24.,-15.));
#17751=CARTESIAN_POINT('Origin',(0.,24.,0.));
#17752=CARTESIAN_POINT('Origin',(0.,0.,0.));
#17753=CARTESIAN_POINT('',(0.,20.,-20.));
#17754=CARTESIAN_POINT('',(-2.44929359829471E-15,20.,20.));
#17755=CARTESIAN_POINT('Origin',(0.,20.,0.));
#17756=CARTESIAN_POINT('',(-2.44929359829471E-15,0.,20.));
#17757=CARTESIAN_POINT('Origin',(0.,20.,0.));
#17758=CARTESIAN_POINT('Origin',(20.,19.5,0.));
#17759=CARTESIAN_POINT('',(0.,19.5,-19.5));
#17760=CARTESIAN_POINT('Origin',(0.,19.5,0.));
#17761=CARTESIAN_POINT('Origin',(0.,20.8,0.));
#17762=CARTESIAN_POINT('',(-1.83697019872103E-15,20.8,-15.));
#17763=CARTESIAN_POINT('Origin',(0.,20.8,0.));
#17764=CARTESIAN_POINT('',(-1.83697019872103E-15,20.8,-15.));
#17765=CARTESIAN_POINT('Origin',(0.,20.8,0.));
#17766=CARTESIAN_POINT('',(-6.73555739531046E-16,20.8,-5.50000000000002));
#17767=CARTESIAN_POINT('Origin',(0.,20.8,0.));
#17768=CARTESIAN_POINT('',(10.9,20.8,-3.));
#17769=CARTESIAN_POINT('Origin',(10.9,20.8,0.));
#17770=CARTESIAN_POINT('Origin',(0.,1.3,-17.85));
#17771=CARTESIAN_POINT('',(0.,1.3,17.85));
#17772=CARTESIAN_POINT('Origin',(0.,1.3,0.));
#17773=CARTESIAN_POINT('',(-2.02066721859313E-15,1.29999999999999,-16.5));
#17774=CARTESIAN_POINT('Origin',(0.,1.3,0.));
#17775=CARTESIAN_POINT('Origin',(0.,19.5,0.));
#17776=CARTESIAN_POINT('',(-2.02066721859313E-15,2.99999999999999,-16.5));
#17777=CARTESIAN_POINT('Origin',(0.,2.99999999999999,0.));
#17778=CARTESIAN_POINT('',(-2.02066721859313E-15,19.5,-16.5));
#17779=CARTESIAN_POINT('Origin',(0.,3.,-17.85));
#17780=CARTESIAN_POINT('Origin',(17.85,0.,0.));
#17781=CARTESIAN_POINT('',(-2.18599453647803E-15,0.,17.85));
#17782=CARTESIAN_POINT('Origin',(0.,0.,0.));
#17783=CARTESIAN_POINT('Origin',(0.,0.,0.));
#17784=CARTESIAN_POINT('',(-2.18599453647803E-15,0.,17.85));
#17785=CARTESIAN_POINT('Origin',(10.9,6.89999999999999,0.));
#17786=CARTESIAN_POINT('',(10.9,18.1,-3.));
#17787=CARTESIAN_POINT('Origin',(10.9,18.1,0.));
#17788=CARTESIAN_POINT('',(10.9,6.89999999999999,-3.));
#17789=CARTESIAN_POINT('Origin',(0.,6.89999999999999,0.));
#17790=CARTESIAN_POINT('',(-6.12323399573677E-16,6.89999999999999,-5.));
#17791=CARTESIAN_POINT('Origin',(0.,6.89999999999999,0.));
#17792=CARTESIAN_POINT('',(0.,9.79999999999999,-5.));
#17793=CARTESIAN_POINT('',(-6.12323399573677E-16,6.89999999999999,-5.));
#17794=CARTESIAN_POINT('',(-6.98315068203329E-17,18.1,-5.));
#17795=CARTESIAN_POINT('',(2.43989602143332E-17,6.89999999999999,-5.));
#17796=CARTESIAN_POINT('',(-6.12323399573677E-16,20.3,-5.));
#17797=CARTESIAN_POINT('',(-6.12323399573677E-16,6.89999999999999,-5.));
#17798=CARTESIAN_POINT('Origin',(0.,20.3,0.));
#17799=CARTESIAN_POINT('',(-6.98315068203329E-17,18.1,5.));
#17800=CARTESIAN_POINT('Origin',(0.,18.1,0.));
#17801=CARTESIAN_POINT('',(0.,9.79999999999999,5.));
#17802=CARTESIAN_POINT('',(2.43989602143332E-17,6.89999999999999,5.));
#17803=CARTESIAN_POINT('Origin',(0.,9.79999999999999,0.));
#17804=CARTESIAN_POINT('Origin',(0.,6.89999999999999,0.));
#17805=CARTESIAN_POINT('Origin',(17.85,9.8,-20.));
#17806=CARTESIAN_POINT('',(0.,9.79999999999999,-20.));
#17807=CARTESIAN_POINT('',(0.,9.79999999999999,-20.));
#17808=CARTESIAN_POINT('',(10.9,9.79999999999999,-3.));
#17809=CARTESIAN_POINT('Origin',(10.9,9.79999999999999,0.));
#17810=CARTESIAN_POINT('Origin',(-6.98315068203329E-17,18.1,-20.));
#17811=CARTESIAN_POINT('',(-6.98315068203329E-17,18.1,-20.));
#17812=CARTESIAN_POINT('Origin',(-6.98315068203329E-17,18.1,-20.));
#17813=CARTESIAN_POINT('',(-6.98315068203329E-17,18.1,-20.));
#17814=CARTESIAN_POINT('Origin',(17.85,18.1,-20.));
#17815=CARTESIAN_POINT('Origin',(10.9,6.89999999999999,0.));
#17816=CARTESIAN_POINT('',(10.9,6.89999999999999,-3.));
#17817=CARTESIAN_POINT('Origin',(10.9,6.89999999999999,0.));
#17818=CARTESIAN_POINT('Origin',(10.9,6.89999999999999,0.));
#17819=CARTESIAN_POINT('',(10.9,6.89999999999999,-3.));
#17820=CARTESIAN_POINT('Origin',(-3.65,-7.99999999999999,0.));
#17821=CARTESIAN_POINT('',(-3.65,-7.99999999999999,2.8));
#17822=CARTESIAN_POINT('Origin',(-3.65,-7.99999999999999,0.));
#17823=CARTESIAN_POINT('',(-3.65,-7.99999999999999,2.8));
#17824=CARTESIAN_POINT('Origin',(-3.65,-7.99999999999999,0.));
#17825=CARTESIAN_POINT('Origin',(0.,-15.5,0.));
#17826=CARTESIAN_POINT('',(0.,-15.5,-6.08697438789325));
#17827=CARTESIAN_POINT('',(-7.45439370062539E-16,-15.5,-6.08697438789325));
#17828=CARTESIAN_POINT('Origin',(0.,-15.5,0.));
#17829=CARTESIAN_POINT('Origin',(0.,-15.5,0.));
#17830=CARTESIAN_POINT('Origin',(0.,19.5,0.));
#17831=CARTESIAN_POINT('',(-2.38806125833734E-15,19.5,-19.5));
#17832=CARTESIAN_POINT('Origin',(0.,20.3,0.));
#17833=CARTESIAN_POINT('',(-6.12323399573677E-16,20.3,-5.));
#17834=CARTESIAN_POINT('',(0.,0.,0.));
#17835=CARTESIAN_POINT('Origin',(0.,4.,-3.1));
#17836=CARTESIAN_POINT('',(8.7469213123627,4.,-17.7935825296398));
#17837=CARTESIAN_POINT('',(8.7469213123627,-4.,-17.7935825296398));
#17838=CARTESIAN_POINT('',(8.7469213123627,4.,-17.7935825296398));
#17839=CARTESIAN_POINT('',(-8.7469213123627,-4.,-17.7935825296398));
#17840=CARTESIAN_POINT('Origin',(0.,-4.,-3.1));
#17841=CARTESIAN_POINT('',(-8.7469213123627,4.,-17.7935825296398));
#17842=CARTESIAN_POINT('',(-8.7469213123627,4.,-17.7935825296398));
#17843=CARTESIAN_POINT('Origin',(0.,4.,-3.1));
#17844=CARTESIAN_POINT('Origin',(0.,4.,0.));
#17845=CARTESIAN_POINT('',(4.6593991028887,-4.,-7.7));
#17846=CARTESIAN_POINT('',(-4.6593991028887,-4.,-7.7));
#17847=CARTESIAN_POINT('Origin',(0.,-4.,0.));
#17848=CARTESIAN_POINT('',(4.6593991028887,4.,-7.7));
#17849=CARTESIAN_POINT('',(4.6593991028887,4.,-7.7));
#17850=CARTESIAN_POINT('',(-4.6593991028887,4.,-7.7));
#17851=CARTESIAN_POINT('Origin',(0.,4.,0.));
#17852=CARTESIAN_POINT('',(-4.6593991028887,4.,-7.7));
#17853=CARTESIAN_POINT('Origin',(4.6593991028887,4.,-7.7));
#17854=CARTESIAN_POINT('',(15.8596026089922,-4.,-9.49398194279967));
#17855=CARTESIAN_POINT('',(4.6593991028887,-4.,-7.7));
#17856=CARTESIAN_POINT('',(15.8596026089922,4.,-9.49398194279967));
#17857=CARTESIAN_POINT('',(15.8596026089922,4.,-9.49398194279967));
#17858=CARTESIAN_POINT('',(4.6593991028887,4.,-7.7));
#17859=CARTESIAN_POINT('Origin',(-15.8596026089922,4.,-9.49398194279967));
#17860=CARTESIAN_POINT('',(-15.8596026089922,-4.,-9.49398194279967));
#17861=CARTESIAN_POINT('',(-15.8596026089922,-4.,-9.49398194279967));
#17862=CARTESIAN_POINT('',(-15.8596026089922,4.,-9.49398194279967));
#17863=CARTESIAN_POINT('',(-15.8596026089922,4.,-9.49398194279967));
#17864=CARTESIAN_POINT('',(-15.8596026089922,4.,-9.49398194279967));
#17865=CARTESIAN_POINT('Origin',(0.,4.,0.));
#17866=CARTESIAN_POINT('',(16.7042622998248,4.,-11.4711137053999));
#17867=CARTESIAN_POINT('',(9.98182727519893,4.,4.26438303187517));
#17868=CARTESIAN_POINT('',(14.6148366502913,4.,-11.9778685327787));
#17869=CARTESIAN_POINT('',(3.55556121796803,4.,-14.6601086086066));
#17870=CARTESIAN_POINT('',(15.1281735948574,4.,-14.0656868154229));
#17871=CARTESIAN_POINT('',(11.0045483578897,4.,2.7057149931719));
#17872=CARTESIAN_POINT('',(12.9842634503587,4.,-14.227394243563));
#17873=CARTESIAN_POINT('',(1.1405019977285,4.,-15.1207265545853));
#17874=CARTESIAN_POINT('',(13.152726411984,4.,-16.3707841358972));
#17875=CARTESIAN_POINT('',(11.7931885652427,4.,0.926903443844235));
#17876=CARTESIAN_POINT('',(11.0109274142019,4.,-16.1831753591847));
#17877=CARTESIAN_POINT('',(-1.32291530947978,4.,-15.1028045363624));
#17878=CARTESIAN_POINT('',(10.8300692524884,4.,-18.325554953314));
#17879=CARTESIAN_POINT('',(12.2895168970939,4.,-1.03747227636268));
#17880=CARTESIAN_POINT('',(-3.73025667693335,4.,-14.60729197018));
#17881=CARTESIAN_POINT('',(-10.8300692524884,4.,-18.325554953314));
#17882=CARTESIAN_POINT('',(3.73025667693335,4.,-14.60729197018));
#17883=CARTESIAN_POINT('',(-11.0109274142019,4.,-16.1831753591847));
#17884=CARTESIAN_POINT('',(-12.2895168970939,4.,-1.03747227636268));
#17885=CARTESIAN_POINT('',(-13.152726411984,4.,-16.3707841358972));
#17886=CARTESIAN_POINT('',(1.32291530947978,4.,-15.1028045363624));
#17887=CARTESIAN_POINT('',(-12.9842634503587,4.,-14.227394243563));
#17888=CARTESIAN_POINT('',(-11.7931885652427,4.,0.926903443844235));
#17889=CARTESIAN_POINT('',(-15.1281735948574,4.,-14.0656868154229));
#17890=CARTESIAN_POINT('',(-1.1405019977285,4.,-15.1207265545853));
#17891=CARTESIAN_POINT('',(-14.6148366502913,4.,-11.9778685327787));
#17892=CARTESIAN_POINT('',(-11.0045483578897,4.,2.7057149931719));
#17893=CARTESIAN_POINT('',(-16.7042622998248,4.,-11.4711137053999));
#17894=CARTESIAN_POINT('',(-3.55556121796803,4.,-14.6601086086066));
#17895=CARTESIAN_POINT('',(-9.98182727519893,4.,4.26438303187517));
#17896=CARTESIAN_POINT('',(-4.28626379701574E-16,4.,-18.));
#17897=CARTESIAN_POINT('Origin',(0.,4.,-14.5));
#17898=CARTESIAN_POINT('Origin',(0.,-4.,0.));
#17899=CARTESIAN_POINT('',(-16.7042622998248,-4.,-11.4711137053999));
#17900=CARTESIAN_POINT('',(-9.98182727519893,-4.,4.26438303187517));
#17901=CARTESIAN_POINT('',(-14.6148366502913,-4.,-11.9778685327787));
#17902=CARTESIAN_POINT('',(-3.55556121796803,-4.,-14.6601086086066));
#17903=CARTESIAN_POINT('',(-15.1281735948574,-4.,-14.0656868154229));
#17904=CARTESIAN_POINT('',(-11.0045483578897,-4.,2.7057149931719));
#17905=CARTESIAN_POINT('',(-12.9842634503587,-4.,-14.227394243563));
#17906=CARTESIAN_POINT('',(-1.1405019977285,-4.,-15.1207265545853));
#17907=CARTESIAN_POINT('',(-13.152726411984,-4.,-16.3707841358972));
#17908=CARTESIAN_POINT('',(-11.7931885652427,-4.,0.926903443844235));
#17909=CARTESIAN_POINT('',(-11.0109274142019,-4.,-16.1831753591847));
#17910=CARTESIAN_POINT('',(1.32291530947978,-4.,-15.1028045363624));
#17911=CARTESIAN_POINT('',(-10.8300692524884,-4.,-18.325554953314));
#17912=CARTESIAN_POINT('',(-12.2895168970939,-4.,-1.03747227636268));
#17913=CARTESIAN_POINT('',(3.73025667693335,-4.,-14.60729197018));
#17914=CARTESIAN_POINT('',(10.8300692524884,-4.,-18.325554953314));
#17915=CARTESIAN_POINT('',(-3.73025667693335,-4.,-14.60729197018));
#17916=CARTESIAN_POINT('',(11.0109274142019,-4.,-16.1831753591847));
#17917=CARTESIAN_POINT('',(12.2895168970939,-4.,-1.03747227636268));
#17918=CARTESIAN_POINT('',(13.152726411984,-4.,-16.3707841358972));
#17919=CARTESIAN_POINT('',(-1.32291530947978,-4.,-15.1028045363624));
#17920=CARTESIAN_POINT('',(12.9842634503587,-4.,-14.227394243563));
#17921=CARTESIAN_POINT('',(11.7931885652427,-4.,0.926903443844235));
#17922=CARTESIAN_POINT('',(15.1281735948574,-4.,-14.0656868154229));
#17923=CARTESIAN_POINT('',(1.1405019977285,-4.,-15.1207265545853));
#17924=CARTESIAN_POINT('',(14.6148366502913,-4.,-11.9778685327787));
#17925=CARTESIAN_POINT('',(11.0045483578897,-4.,2.7057149931719));
#17926=CARTESIAN_POINT('',(16.7042622998248,-4.,-11.4711137053999));
#17927=CARTESIAN_POINT('',(3.55556121796803,-4.,-14.6601086086066));
#17928=CARTESIAN_POINT('',(9.98182727519893,-4.,4.26438303187517));
#17929=CARTESIAN_POINT('',(0.,-4.,-11.));
#17930=CARTESIAN_POINT('Origin',(0.,-4.,-14.5));
#17931=CARTESIAN_POINT('Origin',(0.,-4.,-14.5));
#17932=CARTESIAN_POINT('',(0.,-3.49999999999999,-11.5));
#17933=CARTESIAN_POINT('',(-3.67394039744206E-16,-3.49999999999999,-17.5));
#17934=CARTESIAN_POINT('Origin',(0.,-3.49999999999999,-14.5));
#17935=CARTESIAN_POINT('',(-3.67394039744206E-16,3.5,-17.5));
#17936=CARTESIAN_POINT('',(-3.67394039744206E-16,-4.,-17.5));
#17937=CARTESIAN_POINT('Origin',(0.,3.5,-14.5));
#17938=CARTESIAN_POINT('Origin',(0.,-3.49999999999999,-14.5));
#17939=CARTESIAN_POINT('Origin',(-9.98182727519893,4.,4.26438303187517));
#17940=CARTESIAN_POINT('',(-16.7042622998248,4.,-11.4711137053999));
#17941=CARTESIAN_POINT('Origin',(-3.55556121796803,4.,-14.6601086086066));
#17942=CARTESIAN_POINT('',(-14.6148366502913,4.,-11.9778685327787));
#17943=CARTESIAN_POINT('Origin',(-11.0045483578897,4.,2.7057149931719));
#17944=CARTESIAN_POINT('',(-15.1281735948574,4.,-14.0656868154229));
#17945=CARTESIAN_POINT('Origin',(-1.1405019977285,4.,-15.1207265545853));
#17946=CARTESIAN_POINT('',(-12.9842634503587,4.,-14.227394243563));
#17947=CARTESIAN_POINT('Origin',(-11.7931885652427,4.,0.926903443844235));
#17948=CARTESIAN_POINT('',(-13.152726411984,4.,-16.3707841358972));
#17949=CARTESIAN_POINT('Origin',(1.32291530947978,4.,-15.1028045363624));
#17950=CARTESIAN_POINT('',(-11.0109274142019,4.,-16.1831753591847));
#17951=CARTESIAN_POINT('Origin',(-12.2895168970939,4.,-1.03747227636268));
#17952=CARTESIAN_POINT('',(-10.8300692524884,4.,-18.325554953314));
#17953=CARTESIAN_POINT('Origin',(3.73025667693335,4.,-14.60729197018));
#17954=CARTESIAN_POINT('Origin',(9.98182727519893,4.,4.26438303187517));
#17955=CARTESIAN_POINT('',(16.7042622998248,4.,-11.4711137053999));
#17956=CARTESIAN_POINT('Origin',(3.55556121796803,4.,-14.6601086086066));
#17957=CARTESIAN_POINT('',(14.6148366502913,4.,-11.9778685327787));
#17958=CARTESIAN_POINT('Origin',(11.0045483578897,4.,2.7057149931719));
#17959=CARTESIAN_POINT('',(15.1281735948574,4.,-14.0656868154229));
#17960=CARTESIAN_POINT('Origin',(1.1405019977285,4.,-15.1207265545853));
#17961=CARTESIAN_POINT('',(12.9842634503587,4.,-14.227394243563));
#17962=CARTESIAN_POINT('Origin',(11.7931885652427,4.,0.926903443844235));
#17963=CARTESIAN_POINT('',(13.152726411984,4.,-16.3707841358972));
#17964=CARTESIAN_POINT('Origin',(-1.32291530947978,4.,-15.1028045363624));
#17965=CARTESIAN_POINT('',(11.0109274142019,4.,-16.1831753591847));
#17966=CARTESIAN_POINT('Origin',(12.2895168970939,4.,-1.03747227636268));
#17967=CARTESIAN_POINT('',(10.8300692524884,4.,-18.325554953314));
#17968=CARTESIAN_POINT('Origin',(-3.73025667693335,4.,-14.60729197018));
#17969=CARTESIAN_POINT('Origin',(0.,-4.,-14.5));
#17970=CARTESIAN_POINT('',(-4.28626379701574E-16,-4.,-11.));
#17971=CARTESIAN_POINT('Origin',(0.,3.5,-14.5));
#17972=CARTESIAN_POINT('',(-3.67394039744206E-16,3.5,-17.5));
#17973=CARTESIAN_POINT('',(0.,0.,0.));
#17974=CARTESIAN_POINT('Origin',(0.,6.95,0.));
#17975=CARTESIAN_POINT('',(0.,-6.45,3.));
#17976=CARTESIAN_POINT('',(-3.67394039744206E-16,-6.45,-3.));
#17977=CARTESIAN_POINT('Origin',(0.,-6.45,0.));
#17978=CARTESIAN_POINT('Origin',(0.,-6.45,0.));
#17979=CARTESIAN_POINT('',(0.,6.45,3.));
#17980=CARTESIAN_POINT('',(-3.67394039744206E-16,6.95,3.));
#17981=CARTESIAN_POINT('Origin',(0.,6.45,0.));
#17982=CARTESIAN_POINT('Origin',(0.,6.95,0.));
#17983=CARTESIAN_POINT('',(0.,6.95,2.5));
#17984=CARTESIAN_POINT('Origin',(0.,6.95,0.));
#17985=CARTESIAN_POINT('Origin',(0.,-6.95,0.));
#17986=CARTESIAN_POINT('',(-3.06161699786838E-16,-6.95,-2.5));
#17987=CARTESIAN_POINT('Origin',(0.,-6.95,0.));
#17988=CARTESIAN_POINT('Origin',(0.,-6.45,0.));
#17989=CARTESIAN_POINT('',(-3.67394039744206E-16,-6.45,-3.));
#17990=CARTESIAN_POINT('Origin',(0.,6.95,0.));
#17991=CARTESIAN_POINT('',(-3.06161699786838E-16,6.95,2.5));
#17992=CARTESIAN_POINT('',(0.,0.,0.));
#17993=CARTESIAN_POINT('Origin',(0.,0.,0.));
#17994=CARTESIAN_POINT('',(0.,0.,-4.50000000000001));
#17995=CARTESIAN_POINT('Origin',(0.,0.,0.));
#17996=CARTESIAN_POINT('Origin',(0.,0.,0.));
#17997=CARTESIAN_POINT('',(0.,0.499999999999993,-5.));
#17998=CARTESIAN_POINT('',(-6.12323399573677E-16,0.499999999999993,5.));
#17999=CARTESIAN_POINT('Origin',(0.,0.499999999999993,0.));
#18000=CARTESIAN_POINT('',(-6.12323399573677E-16,12.9,5.));
#18001=CARTESIAN_POINT('',(-6.12323399573677E-16,0.,5.));
#18002=CARTESIAN_POINT('Origin',(0.,12.9,0.));
#18003=CARTESIAN_POINT('Origin',(0.,0.499999999999993,0.));
#18004=CARTESIAN_POINT('',(4.1424630354416,5.9,-2.8));
#18005=CARTESIAN_POINT('',(4.1424630354416,5.9,2.8));
#18006=CARTESIAN_POINT('Ctrl Pts',(4.1424630354416,5.9,-2.8));
#18007=CARTESIAN_POINT('Ctrl Pts',(4.1424630354416,6.2618023460428,-2.8));
#18008=CARTESIAN_POINT('Ctrl Pts',(4.19489580586978,6.63981714967516,-2.72600153733785));
#18009=CARTESIAN_POINT('Ctrl Pts',(4.36844276781151,7.3260008314647,-2.43822468472126));
#18010=CARTESIAN_POINT('Ctrl Pts',(4.48577042903711,7.63518970310634,-2.22460827153833));
#18011=CARTESIAN_POINT('Ctrl Pts',(4.69633401466985,8.1234771250952,-1.73632084954946));
#18012=CARTESIAN_POINT('Ctrl Pts',(4.80503654476778,8.33790022851277,-1.42678909437522));
#18013=CARTESIAN_POINT('Ctrl Pts',(4.9576268468014,8.62636123824948,-0.738944846559111));
#18014=CARTESIAN_POINT('Ctrl Pts',(5.,8.7,-0.360129947555138));
#18015=CARTESIAN_POINT('Ctrl Pts',(5.,8.7,0.360129947555139));
#18016=CARTESIAN_POINT('Ctrl Pts',(4.9576268468014,8.62636123824948,0.738944846559112));
#18017=CARTESIAN_POINT('Ctrl Pts',(4.80503654476778,8.33790022851277,1.42678909437522));
#18018=CARTESIAN_POINT('Ctrl Pts',(4.69633401466985,8.1234771250952,1.73632084954946));
#18019=CARTESIAN_POINT('Ctrl Pts',(4.48577042903712,7.63518970310634,2.22460827153833));
#18020=CARTESIAN_POINT('Ctrl Pts',(4.36844276781151,7.3260008314647,2.43822468472126));
#18021=CARTESIAN_POINT('Ctrl Pts',(4.19489580586978,6.63981714967516,2.72600153733785));
#18022=CARTESIAN_POINT('Ctrl Pts',(4.1424630354416,6.2618023460428,2.8));
#18023=CARTESIAN_POINT('Ctrl Pts',(4.1424630354416,5.9,2.8));
#18024=CARTESIAN_POINT('Ctrl Pts',(4.1424630354416,5.9,2.8));
#18025=CARTESIAN_POINT('Ctrl Pts',(4.1424630354416,5.5381976539572,2.8));
#18026=CARTESIAN_POINT('Ctrl Pts',(4.19489580586978,5.16018285032483,2.72600153733785));
#18027=CARTESIAN_POINT('Ctrl Pts',(4.36844276781151,4.4739991685353,2.43822468472126));
#18028=CARTESIAN_POINT('Ctrl Pts',(4.48577042903712,4.16481029689366,2.22460827153833));
#18029=CARTESIAN_POINT('Ctrl Pts',(4.69633401466985,3.67652287490479,1.73632084954946));
#18030=CARTESIAN_POINT('Ctrl Pts',(4.80503654476778,3.46209977148723,1.42678909437522));
#18031=CARTESIAN_POINT('Ctrl Pts',(4.9576268468014,3.17363876175052,0.73894484655911));
#18032=CARTESIAN_POINT('Ctrl Pts',(5.,3.1,0.360129947555138));
#18033=CARTESIAN_POINT('Ctrl Pts',(5.,3.1,-0.360129947555139));
#18034=CARTESIAN_POINT('Ctrl Pts',(4.9576268468014,3.17363876175052,-0.738944846559111));
#18035=CARTESIAN_POINT('Ctrl Pts',(4.80503654476778,3.46209977148723,-1.42678909437522));
#18036=CARTESIAN_POINT('Ctrl Pts',(4.69633401466985,3.67652287490479,-1.73632084954946));
#18037=CARTESIAN_POINT('Ctrl Pts',(4.48577042903711,4.16481029689366,-2.22460827153833));
#18038=CARTESIAN_POINT('Ctrl Pts',(4.36844276781151,4.4739991685353,-2.43822468472126));
#18039=CARTESIAN_POINT('Ctrl Pts',(4.19489580586978,5.16018285032483,-2.72600153733785));
#18040=CARTESIAN_POINT('Ctrl Pts',(4.1424630354416,5.5381976539572,-2.8));
#18041=CARTESIAN_POINT('Ctrl Pts',(4.1424630354416,5.9,-2.8));
#18042=CARTESIAN_POINT('Origin',(5.,12.9,0.));
#18043=CARTESIAN_POINT('',(0.,12.9,-14.5));
#18044=CARTESIAN_POINT('Origin',(0.,12.9,0.));
#18045=CARTESIAN_POINT('Origin',(0.,0.,0.));
#18046=CARTESIAN_POINT('',(0.,13.4,-15.));
#18047=CARTESIAN_POINT('',(-1.83697019872103E-15,13.4,15.));
#18048=CARTESIAN_POINT('Origin',(0.,13.4,0.));
#18049=CARTESIAN_POINT('',(-1.83697019872103E-15,15.9,15.));
#18050=CARTESIAN_POINT('',(-1.83697019872103E-15,0.,15.));
#18051=CARTESIAN_POINT('Origin',(0.,15.9,0.));
#18052=CARTESIAN_POINT('Origin',(0.,13.4,0.));
#18053=CARTESIAN_POINT('Origin',(15.,15.9,0.));
#18054=CARTESIAN_POINT('',(-12.2997907907885,15.9,-2.22826086956522));
#18055=CARTESIAN_POINT('',(-12.2997907907885,15.9,2.22826086956522));
#18056=CARTESIAN_POINT('Origin',(0.,15.9,0.));
#18057=CARTESIAN_POINT('',(-11.3158075275254,15.9,-3.05));
#18058=CARTESIAN_POINT('Origin',(-11.3158075275254,15.9,-2.05));
#18059=CARTESIAN_POINT('',(11.3158075275254,15.9,-3.05));
#18060=CARTESIAN_POINT('',(-12.1221903961289,15.9,-3.05));
#18061=CARTESIAN_POINT('',(12.2997907907885,15.9,-2.22826086956522));
#18062=CARTESIAN_POINT('Origin',(11.3158075275254,15.9,-2.05));
#18063=CARTESIAN_POINT('',(12.2997907907885,15.9,2.22826086956522));
#18064=CARTESIAN_POINT('Origin',(0.,15.9,0.));
#18065=CARTESIAN_POINT('',(11.3158075275254,15.9,3.05));
#18066=CARTESIAN_POINT('Origin',(11.3158075275254,15.9,2.05));
#18067=CARTESIAN_POINT('',(-11.3158075275254,15.9,3.05));
#18068=CARTESIAN_POINT('',(-12.1221903961289,15.9,3.05));
#18069=CARTESIAN_POINT('Origin',(-11.3158075275254,15.9,2.05));
#18070=CARTESIAN_POINT('Origin',(0.,20.9,0.));
#18071=CARTESIAN_POINT('',(-12.2997907907885,20.9,-2.22826086956522));
#18072=CARTESIAN_POINT('',(-12.2997907907885,20.9,2.22826086956522));
#18073=CARTESIAN_POINT('Origin',(0.,20.9,0.));
#18074=CARTESIAN_POINT('',(-12.2997907907885,20.9,-2.22826086956522));
#18075=CARTESIAN_POINT('',(-12.2997907907885,20.9,2.22826086956522));
#18076=CARTESIAN_POINT('Origin',(-12.1221903961289,20.9,3.05));
#18077=CARTESIAN_POINT('',(11.3158075275254,20.9,3.05));
#18078=CARTESIAN_POINT('',(11.3158075275254,20.9,3.05));
#18079=CARTESIAN_POINT('',(-11.3158075275254,20.9,3.05));
#18080=CARTESIAN_POINT('',(-12.1221903961289,20.9,3.05));
#18081=CARTESIAN_POINT('',(-11.3158075275254,20.9,3.05));
#18082=CARTESIAN_POINT('Origin',(0.,20.9,0.));
#18083=CARTESIAN_POINT('',(12.2997907907885,20.9,-2.22826086956522));
#18084=CARTESIAN_POINT('',(12.2997907907885,20.9,-2.22826086956522));
#18085=CARTESIAN_POINT('',(12.2997907907885,20.9,2.22826086956522));
#18086=CARTESIAN_POINT('Origin',(0.,20.9,0.));
#18087=CARTESIAN_POINT('',(12.2997907907885,20.9,2.22826086956522));
#18088=CARTESIAN_POINT('Origin',(-12.1221903961289,20.9,-3.05));
#18089=CARTESIAN_POINT('',(-11.3158075275254,20.9,-3.05));
#18090=CARTESIAN_POINT('',(-11.3158075275254,20.9,-3.05));
#18091=CARTESIAN_POINT('',(11.3158075275254,20.9,-3.05));
#18092=CARTESIAN_POINT('',(-12.1221903961289,20.9,-3.05));
#18093=CARTESIAN_POINT('',(11.3158075275254,20.9,-3.05));
#18094=CARTESIAN_POINT('Origin',(0.,20.9,0.));
#18095=CARTESIAN_POINT('Origin',(-11.3158075275254,20.9,-2.05));
#18096=CARTESIAN_POINT('Origin',(-11.3158075275254,20.9,2.05));
#18097=CARTESIAN_POINT('Origin',(11.3158075275254,20.9,2.05));
#18098=CARTESIAN_POINT('Origin',(11.3158075275254,20.9,-2.05));
#18099=CARTESIAN_POINT('Origin',(-2.5,5.9,0.));
#18100=CARTESIAN_POINT('',(-2.5,5.9,2.8));
#18101=CARTESIAN_POINT('Origin',(-2.5,5.9,0.));
#18102=CARTESIAN_POINT('',(-2.5,5.9,2.8));
#18103=CARTESIAN_POINT('Origin',(-2.5,5.9,0.));
#18104=CARTESIAN_POINT('Origin',(0.,0.,0.));
#18105=CARTESIAN_POINT('',(-5.5109105961631E-16,0.,-4.50000000000001));
#18106=CARTESIAN_POINT('Origin',(0.,12.9,0.));
#18107=CARTESIAN_POINT('',(-1.77573785876366E-15,12.9,-14.5));
#18108=CARTESIAN_POINT('Origin',(-11.3158075275254,20.9,-2.05));
#18109=CARTESIAN_POINT('Origin',(11.3158075275254,20.9,-2.05));
#18110=CARTESIAN_POINT('Origin',(11.3158075275254,20.9,2.05));
#18111=CARTESIAN_POINT('Origin',(-11.3158075275254,20.9,2.05));
#18112=CARTESIAN_POINT('',(0.,0.,0.));
#18113=CARTESIAN_POINT('Ctrl Pts',(0.,0.,1.8));
#18114=CARTESIAN_POINT('Ctrl Pts',(-1.03923048454133,0.0583333333333332,
1.8));
#18115=CARTESIAN_POINT('Ctrl Pts',(-1.55884572681199,0.116666666666666,
0.9));
#18116=CARTESIAN_POINT('Ctrl Pts',(-2.07846096908265,0.175,1.27269028646989E-16));
#18117=CARTESIAN_POINT('Ctrl Pts',(-1.55884572681199,0.233333333333333,
-0.9));
#18118=CARTESIAN_POINT('Ctrl Pts',(-1.03923048454133,0.291666666666666,
-1.8));
#18119=CARTESIAN_POINT('Ctrl Pts',(-2.20436423846524E-16,0.349999999999999,
-1.8));
#18120=CARTESIAN_POINT('Ctrl Pts',(1.03923048454133,0.408333333333333,-1.8));
#18121=CARTESIAN_POINT('Ctrl Pts',(1.55884572681199,0.466666666666666,-0.900000000000001));
#18122=CARTESIAN_POINT('Ctrl Pts',(2.07846096908265,0.524999999999999,-3.81807085940967E-16));
#18123=CARTESIAN_POINT('Ctrl Pts',(1.55884572681199,0.583333333333332,0.899999999999999));
#18124=CARTESIAN_POINT('Ctrl Pts',(1.03923048454133,0.641666666666665,1.8));
#18125=CARTESIAN_POINT('Ctrl Pts',(0.,0.699999999999999,1.8));
#18126=CARTESIAN_POINT('Ctrl Pts',(-1.03923048454133,0.758333333333332,
1.8));
#18127=CARTESIAN_POINT('Ctrl Pts',(-1.55884572681199,0.816666666666665,
0.9));
#18128=CARTESIAN_POINT('Ctrl Pts',(-2.07846096908265,0.874999999999998,
1.27269028646989E-16));
#18129=CARTESIAN_POINT('Ctrl Pts',(-1.55884572681199,0.933333333333332,
-0.9));
#18130=CARTESIAN_POINT('Ctrl Pts',(-1.03923048454133,0.991666666666665,
-1.8));
#18131=CARTESIAN_POINT('Ctrl Pts',(-2.20436423846524E-16,1.05,-1.8));
#18132=CARTESIAN_POINT('Ctrl Pts',(1.03923048454133,1.10833333333333,-1.8));
#18133=CARTESIAN_POINT('Ctrl Pts',(1.55884572681199,1.16666666666666,-0.900000000000001));
#18134=CARTESIAN_POINT('Ctrl Pts',(2.07846096908265,1.225,-3.81807085940967E-16));
#18135=CARTESIAN_POINT('Ctrl Pts',(1.55884572681199,1.28333333333333,0.899999999999999));
#18136=CARTESIAN_POINT('Ctrl Pts',(1.03923048454133,1.34166666666666,1.8));
#18137=CARTESIAN_POINT('Ctrl Pts',(0.,1.4,1.8));
#18138=CARTESIAN_POINT('Ctrl Pts',(-1.03923048454133,1.45833333333333,1.8));
#18139=CARTESIAN_POINT('Ctrl Pts',(-1.55884572681199,1.51666666666666,0.9));
#18140=CARTESIAN_POINT('Ctrl Pts',(-2.07846096908265,1.575,1.27269028646989E-16));
#18141=CARTESIAN_POINT('Ctrl Pts',(-1.55884572681199,1.63333333333333,-0.9));
#18142=CARTESIAN_POINT('Ctrl Pts',(-1.03923048454133,1.69166666666666,-1.8));
#18143=CARTESIAN_POINT('Ctrl Pts',(-2.20436423846524E-16,1.75,-1.8));
#18144=CARTESIAN_POINT('Ctrl Pts',(1.03923048454133,1.80833333333333,-1.8));
#18145=CARTESIAN_POINT('Ctrl Pts',(1.55884572681199,1.86666666666666,-0.900000000000001));
#18146=CARTESIAN_POINT('Ctrl Pts',(2.07846096908265,1.925,-3.81807085940967E-16));
#18147=CARTESIAN_POINT('Ctrl Pts',(1.55884572681199,1.98333333333333,0.899999999999999));
#18148=CARTESIAN_POINT('Ctrl Pts',(1.03923048454133,2.04166666666666,1.8));
#18149=CARTESIAN_POINT('Ctrl Pts',(0.,2.1,1.8));
#18150=CARTESIAN_POINT('Ctrl Pts',(-1.03923048454133,2.15833333333333,1.8));
#18151=CARTESIAN_POINT('Ctrl Pts',(-1.55884572681199,2.21666666666666,0.9));
#18152=CARTESIAN_POINT('Ctrl Pts',(-2.07846096908265,2.275,1.27269028646989E-16));
#18153=CARTESIAN_POINT('Ctrl Pts',(-1.55884572681199,2.33333333333333,-0.9));
#18154=CARTESIAN_POINT('Ctrl Pts',(-1.03923048454133,2.39166666666666,-1.8));
#18155=CARTESIAN_POINT('Ctrl Pts',(-2.20436423846524E-16,2.45,-1.8));
#18156=CARTESIAN_POINT('Ctrl Pts',(1.03923048454133,2.50833333333333,-1.8));
#18157=CARTESIAN_POINT('Ctrl Pts',(1.55884572681199,2.56666666666666,-0.900000000000001));
#18158=CARTESIAN_POINT('Ctrl Pts',(2.07846096908265,2.62499999999999,-3.81807085940967E-16));
#18159=CARTESIAN_POINT('Ctrl Pts',(1.55884572681199,2.68333333333333,0.899999999999999));
#18160=CARTESIAN_POINT('Ctrl Pts',(1.03923048454133,2.74166666666666,1.8));
#18161=CARTESIAN_POINT('Ctrl Pts',(0.,2.79999999999999,1.8));
#18162=CARTESIAN_POINT('Ctrl Pts',(-1.03923048454133,2.85833333333333,1.8));
#18163=CARTESIAN_POINT('Ctrl Pts',(-1.55884572681199,2.91666666666666,0.9));
#18164=CARTESIAN_POINT('Ctrl Pts',(-2.07846096908265,2.97499999999999,1.27269028646989E-16));
#18165=CARTESIAN_POINT('Ctrl Pts',(-1.55884572681199,3.03333333333333,-0.9));
#18166=CARTESIAN_POINT('Ctrl Pts',(-1.03923048454133,3.09166666666666,-1.8));
#18167=CARTESIAN_POINT('Ctrl Pts',(-2.20436423846524E-16,3.14999999999999,
-1.8));
#18168=CARTESIAN_POINT('Ctrl Pts',(1.03923048454133,3.20833333333333,-1.8));
#18169=CARTESIAN_POINT('Ctrl Pts',(1.55884572681199,3.26666666666666,-0.900000000000001));
#18170=CARTESIAN_POINT('Ctrl Pts',(2.07846096908265,3.32499999999999,-3.81807085940967E-16));
#18171=CARTESIAN_POINT('Ctrl Pts',(1.55884572681199,3.38333333333333,0.899999999999999));
#18172=CARTESIAN_POINT('Ctrl Pts',(1.03923048454133,3.44166666666666,1.8));
#18173=CARTESIAN_POINT('Ctrl Pts',(0.,3.49999999999999,1.8));
#18174=CARTESIAN_POINT('Ctrl Pts',(-1.03923048454133,3.55833333333333,1.8));
#18175=CARTESIAN_POINT('Ctrl Pts',(-1.55884572681199,3.61666666666666,0.9));
#18176=CARTESIAN_POINT('Ctrl Pts',(-2.07846096908265,3.67499999999999,1.27269028646989E-16));
#18177=CARTESIAN_POINT('Ctrl Pts',(-1.55884572681199,3.73333333333333,-0.9));
#18178=CARTESIAN_POINT('Ctrl Pts',(-1.03923048454133,3.79166666666666,-1.8));
#18179=CARTESIAN_POINT('Ctrl Pts',(-2.20436423846524E-16,3.84999999999999,
-1.8));
#18180=CARTESIAN_POINT('Ctrl Pts',(1.03923048454133,3.90833333333333,-1.8));
#18181=CARTESIAN_POINT('Ctrl Pts',(1.55884572681199,3.96666666666666,-0.900000000000001));
#18182=CARTESIAN_POINT('Ctrl Pts',(2.07846096908265,4.02499999999999,-3.81807085940967E-16));
#18183=CARTESIAN_POINT('Ctrl Pts',(1.55884572681199,4.08333333333333,0.899999999999999));
#18184=CARTESIAN_POINT('Ctrl Pts',(1.03923048454133,4.14166666666666,1.8));
#18185=CARTESIAN_POINT('Ctrl Pts',(0.,4.19999999999999,1.8));
#18186=CARTESIAN_POINT('Ctrl Pts',(0.,0.205025253169417,1.8));
#18187=CARTESIAN_POINT('Ctrl Pts',(-1.03923048454133,0.26335858650275,1.8));
#18188=CARTESIAN_POINT('Ctrl Pts',(-1.55884572681199,0.321691919836083,
0.9));
#18189=CARTESIAN_POINT('Ctrl Pts',(-2.07846096908265,0.380025253169416,
1.27269028646989E-16));
#18190=CARTESIAN_POINT('Ctrl Pts',(-1.55884572681199,0.43835858650275,-0.9));
#18191=CARTESIAN_POINT('Ctrl Pts',(-1.03923048454133,0.496691919836083,
-1.8));
#18192=CARTESIAN_POINT('Ctrl Pts',(-2.20436423846524E-16,0.555025253169416,
-1.8));
#18193=CARTESIAN_POINT('Ctrl Pts',(1.03923048454133,0.613358586502749,-1.8));
#18194=CARTESIAN_POINT('Ctrl Pts',(1.55884572681199,0.671691919836083,-0.900000000000001));
#18195=CARTESIAN_POINT('Ctrl Pts',(2.07846096908265,0.730025253169416,-3.81807085940967E-16));
#18196=CARTESIAN_POINT('Ctrl Pts',(1.55884572681199,0.788358586502749,0.899999999999999));
#18197=CARTESIAN_POINT('Ctrl Pts',(1.03923048454133,0.846691919836082,1.8));
#18198=CARTESIAN_POINT('Ctrl Pts',(0.,0.905025253169415,1.8));
#18199=CARTESIAN_POINT('Ctrl Pts',(-1.03923048454133,0.963358586502749,
1.8));
#18200=CARTESIAN_POINT('Ctrl Pts',(-1.55884572681199,1.02169191983608,0.9));
#18201=CARTESIAN_POINT('Ctrl Pts',(-2.07846096908265,1.08002525316942,1.27269028646989E-16));
#18202=CARTESIAN_POINT('Ctrl Pts',(-1.55884572681199,1.13835858650275,-0.9));
#18203=CARTESIAN_POINT('Ctrl Pts',(-1.03923048454133,1.19669191983608,-1.8));
#18204=CARTESIAN_POINT('Ctrl Pts',(-2.20436423846524E-16,1.25502525316941,
-1.8));
#18205=CARTESIAN_POINT('Ctrl Pts',(1.03923048454133,1.31335858650275,-1.8));
#18206=CARTESIAN_POINT('Ctrl Pts',(1.55884572681199,1.37169191983608,-0.900000000000001));
#18207=CARTESIAN_POINT('Ctrl Pts',(2.07846096908265,1.43002525316941,-3.81807085940967E-16));
#18208=CARTESIAN_POINT('Ctrl Pts',(1.55884572681199,1.48835858650275,0.899999999999999));
#18209=CARTESIAN_POINT('Ctrl Pts',(1.03923048454133,1.54669191983608,1.8));
#18210=CARTESIAN_POINT('Ctrl Pts',(0.,1.60502525316941,1.8));
#18211=CARTESIAN_POINT('Ctrl Pts',(-1.03923048454133,1.66335858650275,1.8));
#18212=CARTESIAN_POINT('Ctrl Pts',(-1.55884572681199,1.72169191983608,0.9));
#18213=CARTESIAN_POINT('Ctrl Pts',(-2.07846096908265,1.78002525316941,1.27269028646989E-16));
#18214=CARTESIAN_POINT('Ctrl Pts',(-1.55884572681199,1.83835858650275,-0.9));
#18215=CARTESIAN_POINT('Ctrl Pts',(-1.03923048454133,1.89669191983608,-1.8));
#18216=CARTESIAN_POINT('Ctrl Pts',(-2.20436423846524E-16,1.95502525316941,
-1.8));
#18217=CARTESIAN_POINT('Ctrl Pts',(1.03923048454133,2.01335858650275,-1.8));
#18218=CARTESIAN_POINT('Ctrl Pts',(1.55884572681199,2.07169191983608,-0.900000000000001));
#18219=CARTESIAN_POINT('Ctrl Pts',(2.07846096908265,2.13002525316941,-3.81807085940967E-16));
#18220=CARTESIAN_POINT('Ctrl Pts',(1.55884572681199,2.18835858650275,0.899999999999999));
#18221=CARTESIAN_POINT('Ctrl Pts',(1.03923048454133,2.24669191983608,1.8));
#18222=CARTESIAN_POINT('Ctrl Pts',(0.,2.30502525316941,1.8));
#18223=CARTESIAN_POINT('Ctrl Pts',(-1.03923048454133,2.36335858650275,1.8));
#18224=CARTESIAN_POINT('Ctrl Pts',(-1.55884572681199,2.42169191983608,0.9));
#18225=CARTESIAN_POINT('Ctrl Pts',(-2.07846096908265,2.48002525316941,1.27269028646989E-16));
#18226=CARTESIAN_POINT('Ctrl Pts',(-1.55884572681199,2.53835858650275,-0.9));
#18227=CARTESIAN_POINT('Ctrl Pts',(-1.03923048454133,2.59669191983608,-1.8));
#18228=CARTESIAN_POINT('Ctrl Pts',(-2.20436423846524E-16,2.65502525316941,
-1.8));
#18229=CARTESIAN_POINT('Ctrl Pts',(1.03923048454133,2.71335858650274,-1.8));
#18230=CARTESIAN_POINT('Ctrl Pts',(1.55884572681199,2.77169191983608,-0.900000000000001));
#18231=CARTESIAN_POINT('Ctrl Pts',(2.07846096908265,2.83002525316941,-3.81807085940967E-16));
#18232=CARTESIAN_POINT('Ctrl Pts',(1.55884572681199,2.88835858650274,0.899999999999999));
#18233=CARTESIAN_POINT('Ctrl Pts',(1.03923048454133,2.94669191983608,1.8));
#18234=CARTESIAN_POINT('Ctrl Pts',(0.,3.00502525316941,1.8));
#18235=CARTESIAN_POINT('Ctrl Pts',(-1.03923048454133,3.06335858650274,1.8));
#18236=CARTESIAN_POINT('Ctrl Pts',(-1.55884572681199,3.12169191983608,0.9));
#18237=CARTESIAN_POINT('Ctrl Pts',(-2.07846096908265,3.18002525316941,1.27269028646989E-16));
#18238=CARTESIAN_POINT('Ctrl Pts',(-1.55884572681199,3.23835858650274,-0.9));
#18239=CARTESIAN_POINT('Ctrl Pts',(-1.03923048454133,3.29669191983608,-1.8));
#18240=CARTESIAN_POINT('Ctrl Pts',(-2.20436423846524E-16,3.35502525316941,
-1.8));
#18241=CARTESIAN_POINT('Ctrl Pts',(1.03923048454133,3.41335858650274,-1.8));
#18242=CARTESIAN_POINT('Ctrl Pts',(1.55884572681199,3.47169191983608,-0.900000000000001));
#18243=CARTESIAN_POINT('Ctrl Pts',(2.07846096908265,3.53002525316941,-3.81807085940967E-16));
#18244=CARTESIAN_POINT('Ctrl Pts',(1.55884572681199,3.58835858650274,0.899999999999999));
#18245=CARTESIAN_POINT('Ctrl Pts',(1.03923048454133,3.64669191983608,1.8));
#18246=CARTESIAN_POINT('Ctrl Pts',(0.,3.70502525316941,1.8));
#18247=CARTESIAN_POINT('Ctrl Pts',(-1.03923048454133,3.76335858650274,1.8));
#18248=CARTESIAN_POINT('Ctrl Pts',(-1.55884572681199,3.82169191983608,0.9));
#18249=CARTESIAN_POINT('Ctrl Pts',(-2.07846096908265,3.88002525316941,1.27269028646989E-16));
#18250=CARTESIAN_POINT('Ctrl Pts',(-1.55884572681199,3.93835858650274,-0.9));
#18251=CARTESIAN_POINT('Ctrl Pts',(-1.03923048454133,3.99669191983608,-1.8));
#18252=CARTESIAN_POINT('Ctrl Pts',(-2.20436423846524E-16,4.05502525316941,
-1.8));
#18253=CARTESIAN_POINT('Ctrl Pts',(1.03923048454133,4.11335858650274,-1.8));
#18254=CARTESIAN_POINT('Ctrl Pts',(1.55884572681199,4.17169191983608,-0.900000000000001));
#18255=CARTESIAN_POINT('Ctrl Pts',(2.07846096908265,4.23002525316941,-3.81807085940967E-16));
#18256=CARTESIAN_POINT('Ctrl Pts',(1.55884572681199,4.28835858650274,0.899999999999999));
#18257=CARTESIAN_POINT('Ctrl Pts',(1.03923048454133,4.34669191983608,1.8));
#18258=CARTESIAN_POINT('Ctrl Pts',(0.,4.40502525316941,1.8));
#18259=CARTESIAN_POINT('Ctrl Pts',(0.,0.35,1.94497474683058));
#18260=CARTESIAN_POINT('Ctrl Pts',(-1.12293169364966,0.408333333333333,
1.94497474683058));
#18261=CARTESIAN_POINT('Ctrl Pts',(-1.68439754047449,0.466666666666666,
0.972487373415292));
#18262=CARTESIAN_POINT('Ctrl Pts',(-2.24586338729932,0.525,1.37519470428917E-16));
#18263=CARTESIAN_POINT('Ctrl Pts',(-1.68439754047449,0.583333333333333,
-0.972487373415291));
#18264=CARTESIAN_POINT('Ctrl Pts',(-1.12293169364966,0.641666666666666,
-1.94497474683058));
#18265=CARTESIAN_POINT('Ctrl Pts',(-2.38190709812851E-16,0.699999999999999,
-1.94497474683058));
#18266=CARTESIAN_POINT('Ctrl Pts',(1.12293169364966,0.758333333333333,-1.94497474683058));
#18267=CARTESIAN_POINT('Ctrl Pts',(1.68439754047449,0.816666666666666,-0.972487373415292));
#18268=CARTESIAN_POINT('Ctrl Pts',(2.24586338729932,0.874999999999999,-4.12558411286752E-16));
#18269=CARTESIAN_POINT('Ctrl Pts',(1.68439754047449,0.933333333333332,0.97248737341529));
#18270=CARTESIAN_POINT('Ctrl Pts',(1.12293169364966,0.991666666666665,1.94497474683058));
#18271=CARTESIAN_POINT('Ctrl Pts',(0.,1.05,1.94497474683058));
#18272=CARTESIAN_POINT('Ctrl Pts',(-1.12293169364966,1.10833333333333,1.94497474683058));
#18273=CARTESIAN_POINT('Ctrl Pts',(-1.68439754047449,1.16666666666666,0.972487373415292));
#18274=CARTESIAN_POINT('Ctrl Pts',(-2.24586338729932,1.225,1.37519470428917E-16));
#18275=CARTESIAN_POINT('Ctrl Pts',(-1.68439754047449,1.28333333333333,-0.972487373415291));
#18276=CARTESIAN_POINT('Ctrl Pts',(-1.12293169364966,1.34166666666667,-1.94497474683058));
#18277=CARTESIAN_POINT('Ctrl Pts',(-2.38190709812851E-16,1.4,-1.94497474683058));
#18278=CARTESIAN_POINT('Ctrl Pts',(1.12293169364966,1.45833333333333,-1.94497474683058));
#18279=CARTESIAN_POINT('Ctrl Pts',(1.68439754047449,1.51666666666666,-0.972487373415292));
#18280=CARTESIAN_POINT('Ctrl Pts',(2.24586338729932,1.575,-4.12558411286752E-16));
#18281=CARTESIAN_POINT('Ctrl Pts',(1.68439754047449,1.63333333333333,0.97248737341529));
#18282=CARTESIAN_POINT('Ctrl Pts',(1.12293169364966,1.69166666666666,1.94497474683058));
#18283=CARTESIAN_POINT('Ctrl Pts',(0.,1.75,1.94497474683058));
#18284=CARTESIAN_POINT('Ctrl Pts',(-1.12293169364966,1.80833333333333,1.94497474683058));
#18285=CARTESIAN_POINT('Ctrl Pts',(-1.68439754047449,1.86666666666666,0.972487373415292));
#18286=CARTESIAN_POINT('Ctrl Pts',(-2.24586338729932,1.925,1.37519470428917E-16));
#18287=CARTESIAN_POINT('Ctrl Pts',(-1.68439754047449,1.98333333333333,-0.972487373415291));
#18288=CARTESIAN_POINT('Ctrl Pts',(-1.12293169364966,2.04166666666666,-1.94497474683058));
#18289=CARTESIAN_POINT('Ctrl Pts',(-2.38190709812851E-16,2.1,-1.94497474683058));
#18290=CARTESIAN_POINT('Ctrl Pts',(1.12293169364966,2.15833333333333,-1.94497474683058));
#18291=CARTESIAN_POINT('Ctrl Pts',(1.68439754047449,2.21666666666666,-0.972487373415292));
#18292=CARTESIAN_POINT('Ctrl Pts',(2.24586338729932,2.275,-4.12558411286752E-16));
#18293=CARTESIAN_POINT('Ctrl Pts',(1.68439754047449,2.33333333333333,0.97248737341529));
#18294=CARTESIAN_POINT('Ctrl Pts',(1.12293169364966,2.39166666666666,1.94497474683058));
#18295=CARTESIAN_POINT('Ctrl Pts',(0.,2.45,1.94497474683058));
#18296=CARTESIAN_POINT('Ctrl Pts',(-1.12293169364966,2.50833333333333,1.94497474683058));
#18297=CARTESIAN_POINT('Ctrl Pts',(-1.68439754047449,2.56666666666666,0.972487373415292));
#18298=CARTESIAN_POINT('Ctrl Pts',(-2.24586338729932,2.62499999999999,1.37519470428917E-16));
#18299=CARTESIAN_POINT('Ctrl Pts',(-1.68439754047449,2.68333333333333,-0.972487373415291));
#18300=CARTESIAN_POINT('Ctrl Pts',(-1.12293169364966,2.74166666666666,-1.94497474683058));
#18301=CARTESIAN_POINT('Ctrl Pts',(-2.38190709812851E-16,2.8,-1.94497474683058));
#18302=CARTESIAN_POINT('Ctrl Pts',(1.12293169364966,2.85833333333333,-1.94497474683058));
#18303=CARTESIAN_POINT('Ctrl Pts',(1.68439754047449,2.91666666666666,-0.972487373415292));
#18304=CARTESIAN_POINT('Ctrl Pts',(2.24586338729932,2.97499999999999,-4.12558411286752E-16));
#18305=CARTESIAN_POINT('Ctrl Pts',(1.68439754047449,3.03333333333333,0.97248737341529));
#18306=CARTESIAN_POINT('Ctrl Pts',(1.12293169364966,3.09166666666666,1.94497474683058));
#18307=CARTESIAN_POINT('Ctrl Pts',(0.,3.14999999999999,1.94497474683058));
#18308=CARTESIAN_POINT('Ctrl Pts',(-1.12293169364966,3.20833333333333,1.94497474683058));
#18309=CARTESIAN_POINT('Ctrl Pts',(-1.68439754047449,3.26666666666666,0.972487373415292));
#18310=CARTESIAN_POINT('Ctrl Pts',(-2.24586338729932,3.32499999999999,1.37519470428917E-16));
#18311=CARTESIAN_POINT('Ctrl Pts',(-1.68439754047449,3.38333333333333,-0.972487373415291));
#18312=CARTESIAN_POINT('Ctrl Pts',(-1.12293169364966,3.44166666666666,-1.94497474683058));
#18313=CARTESIAN_POINT('Ctrl Pts',(-2.38190709812851E-16,3.49999999999999,
-1.94497474683058));
#18314=CARTESIAN_POINT('Ctrl Pts',(1.12293169364966,3.55833333333333,-1.94497474683058));
#18315=CARTESIAN_POINT('Ctrl Pts',(1.68439754047449,3.61666666666666,-0.972487373415292));
#18316=CARTESIAN_POINT('Ctrl Pts',(2.24586338729932,3.67499999999999,-4.12558411286752E-16));
#18317=CARTESIAN_POINT('Ctrl Pts',(1.68439754047449,3.73333333333333,0.97248737341529));
#18318=CARTESIAN_POINT('Ctrl Pts',(1.12293169364966,3.79166666666666,1.94497474683058));
#18319=CARTESIAN_POINT('Ctrl Pts',(0.,3.84999999999999,1.94497474683058));
#18320=CARTESIAN_POINT('Ctrl Pts',(-1.12293169364966,3.90833333333333,1.94497474683058));
#18321=CARTESIAN_POINT('Ctrl Pts',(-1.68439754047449,3.96666666666666,0.972487373415292));
#18322=CARTESIAN_POINT('Ctrl Pts',(-2.24586338729932,4.02499999999999,1.37519470428917E-16));
#18323=CARTESIAN_POINT('Ctrl Pts',(-1.68439754047449,4.08333333333333,-0.972487373415291));
#18324=CARTESIAN_POINT('Ctrl Pts',(-1.12293169364966,4.14166666666666,-1.94497474683058));
#18325=CARTESIAN_POINT('Ctrl Pts',(-2.38190709812851E-16,4.19999999999999,
-1.94497474683058));
#18326=CARTESIAN_POINT('Ctrl Pts',(1.12293169364966,4.25833333333332,-1.94497474683058));
#18327=CARTESIAN_POINT('Ctrl Pts',(1.68439754047449,4.31666666666666,-0.972487373415292));
#18328=CARTESIAN_POINT('Ctrl Pts',(2.24586338729932,4.37499999999999,-4.12558411286752E-16));
#18329=CARTESIAN_POINT('Ctrl Pts',(1.68439754047449,4.43333333333332,0.97248737341529));
#18330=CARTESIAN_POINT('Ctrl Pts',(1.12293169364966,4.49166666666666,1.94497474683058));
#18331=CARTESIAN_POINT('Ctrl Pts',(0.,4.54999999999999,1.94497474683058));
#18332=CARTESIAN_POINT('Ctrl Pts',(0.,0.35,2.15));
#18333=CARTESIAN_POINT('Ctrl Pts',(-1.2413030787577,0.408333333333333,2.15));
#18334=CARTESIAN_POINT('Ctrl Pts',(-1.86195461813654,0.466666666666667,
1.075));
#18335=CARTESIAN_POINT('Ctrl Pts',(-2.48260615751539,0.525,1.52015784217237E-16));
#18336=CARTESIAN_POINT('Ctrl Pts',(-1.86195461813654,0.583333333333333,
-1.075));
#18337=CARTESIAN_POINT('Ctrl Pts',(-1.2413030787577,0.641666666666666,-2.15));
#18338=CARTESIAN_POINT('Ctrl Pts',(-2.63299061816681E-16,0.699999999999999,
-2.15));
#18339=CARTESIAN_POINT('Ctrl Pts',(1.24130307875769,0.758333333333333,-2.15));
#18340=CARTESIAN_POINT('Ctrl Pts',(1.86195461813654,0.816666666666666,-1.075));
#18341=CARTESIAN_POINT('Ctrl Pts',(2.48260615751539,0.874999999999999,-4.5604735265171E-16));
#18342=CARTESIAN_POINT('Ctrl Pts',(1.86195461813654,0.933333333333332,1.075));
#18343=CARTESIAN_POINT('Ctrl Pts',(1.2413030787577,0.991666666666666,2.15));
#18344=CARTESIAN_POINT('Ctrl Pts',(0.,1.05,2.15));
#18345=CARTESIAN_POINT('Ctrl Pts',(-1.2413030787577,1.10833333333333,2.15));
#18346=CARTESIAN_POINT('Ctrl Pts',(-1.86195461813654,1.16666666666667,1.075));
#18347=CARTESIAN_POINT('Ctrl Pts',(-2.48260615751539,1.225,1.52015784217237E-16));
#18348=CARTESIAN_POINT('Ctrl Pts',(-1.86195461813654,1.28333333333333,-1.075));
#18349=CARTESIAN_POINT('Ctrl Pts',(-1.2413030787577,1.34166666666666,-2.15));
#18350=CARTESIAN_POINT('Ctrl Pts',(-2.63299061816681E-16,1.4,-2.15));
#18351=CARTESIAN_POINT('Ctrl Pts',(1.24130307875769,1.45833333333333,-2.15));
#18352=CARTESIAN_POINT('Ctrl Pts',(1.86195461813654,1.51666666666666,-1.075));
#18353=CARTESIAN_POINT('Ctrl Pts',(2.48260615751539,1.575,-4.5604735265171E-16));
#18354=CARTESIAN_POINT('Ctrl Pts',(1.86195461813654,1.63333333333333,1.075));
#18355=CARTESIAN_POINT('Ctrl Pts',(1.2413030787577,1.69166666666666,2.15));
#18356=CARTESIAN_POINT('Ctrl Pts',(0.,1.75,2.15));
#18357=CARTESIAN_POINT('Ctrl Pts',(-1.2413030787577,1.80833333333333,2.15));
#18358=CARTESIAN_POINT('Ctrl Pts',(-1.86195461813654,1.86666666666666,1.075));
#18359=CARTESIAN_POINT('Ctrl Pts',(-2.48260615751539,1.925,1.52015784217237E-16));
#18360=CARTESIAN_POINT('Ctrl Pts',(-1.86195461813654,1.98333333333333,-1.075));
#18361=CARTESIAN_POINT('Ctrl Pts',(-1.2413030787577,2.04166666666666,-2.15));
#18362=CARTESIAN_POINT('Ctrl Pts',(-2.63299061816681E-16,2.1,-2.15));
#18363=CARTESIAN_POINT('Ctrl Pts',(1.24130307875769,2.15833333333333,-2.15));
#18364=CARTESIAN_POINT('Ctrl Pts',(1.86195461813654,2.21666666666666,-1.075));
#18365=CARTESIAN_POINT('Ctrl Pts',(2.48260615751539,2.275,-4.5604735265171E-16));
#18366=CARTESIAN_POINT('Ctrl Pts',(1.86195461813654,2.33333333333333,1.075));
#18367=CARTESIAN_POINT('Ctrl Pts',(1.2413030787577,2.39166666666666,2.15));
#18368=CARTESIAN_POINT('Ctrl Pts',(0.,2.45,2.15));
#18369=CARTESIAN_POINT('Ctrl Pts',(-1.2413030787577,2.50833333333333,2.15));
#18370=CARTESIAN_POINT('Ctrl Pts',(-1.86195461813654,2.56666666666666,1.075));
#18371=CARTESIAN_POINT('Ctrl Pts',(-2.48260615751539,2.625,1.52015784217237E-16));
#18372=CARTESIAN_POINT('Ctrl Pts',(-1.86195461813654,2.68333333333333,-1.075));
#18373=CARTESIAN_POINT('Ctrl Pts',(-1.2413030787577,2.74166666666666,-2.15));
#18374=CARTESIAN_POINT('Ctrl Pts',(-2.63299061816681E-16,2.8,-2.15));
#18375=CARTESIAN_POINT('Ctrl Pts',(1.24130307875769,2.85833333333333,-2.15));
#18376=CARTESIAN_POINT('Ctrl Pts',(1.86195461813654,2.91666666666666,-1.075));
#18377=CARTESIAN_POINT('Ctrl Pts',(2.48260615751539,2.97499999999999,-4.5604735265171E-16));
#18378=CARTESIAN_POINT('Ctrl Pts',(1.86195461813654,3.03333333333333,1.075));
#18379=CARTESIAN_POINT('Ctrl Pts',(1.2413030787577,3.09166666666666,2.15));
#18380=CARTESIAN_POINT('Ctrl Pts',(0.,3.15,2.15));
#18381=CARTESIAN_POINT('Ctrl Pts',(-1.2413030787577,3.20833333333333,2.15));
#18382=CARTESIAN_POINT('Ctrl Pts',(-1.86195461813654,3.26666666666666,1.075));
#18383=CARTESIAN_POINT('Ctrl Pts',(-2.48260615751539,3.32499999999999,1.52015784217237E-16));
#18384=CARTESIAN_POINT('Ctrl Pts',(-1.86195461813654,3.38333333333333,-1.075));
#18385=CARTESIAN_POINT('Ctrl Pts',(-1.2413030787577,3.44166666666666,-2.15));
#18386=CARTESIAN_POINT('Ctrl Pts',(-2.63299061816681E-16,3.49999999999999,
-2.15));
#18387=CARTESIAN_POINT('Ctrl Pts',(1.24130307875769,3.55833333333333,-2.15));
#18388=CARTESIAN_POINT('Ctrl Pts',(1.86195461813654,3.61666666666666,-1.075));
#18389=CARTESIAN_POINT('Ctrl Pts',(2.48260615751539,3.67499999999999,-4.5604735265171E-16));
#18390=CARTESIAN_POINT('Ctrl Pts',(1.86195461813654,3.73333333333333,1.075));
#18391=CARTESIAN_POINT('Ctrl Pts',(1.2413030787577,3.79166666666666,2.15));
#18392=CARTESIAN_POINT('Ctrl Pts',(0.,3.84999999999999,2.15));
#18393=CARTESIAN_POINT('Ctrl Pts',(-1.2413030787577,3.90833333333333,2.15));
#18394=CARTESIAN_POINT('Ctrl Pts',(-1.86195461813654,3.96666666666666,1.075));
#18395=CARTESIAN_POINT('Ctrl Pts',(-2.48260615751539,4.02499999999999,1.52015784217237E-16));
#18396=CARTESIAN_POINT('Ctrl Pts',(-1.86195461813654,4.08333333333333,-1.075));
#18397=CARTESIAN_POINT('Ctrl Pts',(-1.2413030787577,4.14166666666666,-2.15));
#18398=CARTESIAN_POINT('Ctrl Pts',(-2.63299061816681E-16,4.19999999999999,
-2.15));
#18399=CARTESIAN_POINT('Ctrl Pts',(1.24130307875769,4.25833333333333,-2.15));
#18400=CARTESIAN_POINT('Ctrl Pts',(1.86195461813654,4.31666666666666,-1.075));
#18401=CARTESIAN_POINT('Ctrl Pts',(2.48260615751539,4.37499999999999,-4.5604735265171E-16));
#18402=CARTESIAN_POINT('Ctrl Pts',(1.86195461813654,4.43333333333333,1.075));
#18403=CARTESIAN_POINT('Ctrl Pts',(1.2413030787577,4.49166666666666,2.15));
#18404=CARTESIAN_POINT('Ctrl Pts',(0.,4.54999999999999,2.15));
#18405=CARTESIAN_POINT('',(-7.40933783759325E-14,4.2,1.8));
#18406=CARTESIAN_POINT('',(-8.82371251094361E-14,4.55,2.15));
#18407=CARTESIAN_POINT('Origin',(-1.80160437084306E-13,4.2,2.15));
#18408=CARTESIAN_POINT('',(-8.87637232330694E-14,3.85,2.15));
#18409=CARTESIAN_POINT('Ctrl Pts',(1.05346240894046E-14,3.84999999999999,
2.15));
#18410=CARTESIAN_POINT('Ctrl Pts',(-1.24130307875769,3.90833333333333,2.15));
#18411=CARTESIAN_POINT('Ctrl Pts',(-1.86195461813654,3.96666666666666,1.075));
#18412=CARTESIAN_POINT('Ctrl Pts',(-2.48260615751539,4.02499999999999,1.67263463193154E-14));
#18413=CARTESIAN_POINT('Ctrl Pts',(-1.86195461813655,4.08333333333333,-1.07499999999999));
#18414=CARTESIAN_POINT('Ctrl Pts',(-1.2413030787577,4.14166666666666,-2.15));
#18415=CARTESIAN_POINT('Ctrl Pts',(-1.07979231512212E-14,4.19999999999999,
-2.15));
#18416=CARTESIAN_POINT('Ctrl Pts',(1.24130307875769,4.25833333333332,-2.15));
#18417=CARTESIAN_POINT('Ctrl Pts',(1.86195461813654,4.31666666666666,-1.07500000000001));
#18418=CARTESIAN_POINT('Ctrl Pts',(2.48260615751539,4.37499999999999,-8.21038903287055E-15));
#18419=CARTESIAN_POINT('Ctrl Pts',(1.86195461813655,4.43333333333332,1.07499999999999));
#18420=CARTESIAN_POINT('Ctrl Pts',(1.24130307875771,4.49166666666666,2.14999999999999));
#18421=CARTESIAN_POINT('Ctrl Pts',(-8.82371251094361E-14,4.55,2.15));
#18422=CARTESIAN_POINT('',(2.63299061816681E-16,0.349999999999999,2.15));
#18423=CARTESIAN_POINT('Ctrl Pts',(2.63299061816681E-16,0.349999999999999,
2.15));
#18424=CARTESIAN_POINT('Ctrl Pts',(-1.24130307875769,0.408333333333333,
2.15));
#18425=CARTESIAN_POINT('Ctrl Pts',(-1.86195461813654,0.466666666666666,
1.075));
#18426=CARTESIAN_POINT('Ctrl Pts',(-2.48260615751539,0.524999999999999,
4.5604735265171E-16));
#18427=CARTESIAN_POINT('Ctrl Pts',(-1.86195461813654,0.583333333333332,
-1.075));
#18428=CARTESIAN_POINT('Ctrl Pts',(-1.2413030787577,0.641666666666665,-2.15));
#18429=CARTESIAN_POINT('Ctrl Pts',(-5.26598123633362E-16,0.699999999999999,
-2.15));
#18430=CARTESIAN_POINT('Ctrl Pts',(1.24130307875769,0.758333333333332,-2.15));
#18431=CARTESIAN_POINT('Ctrl Pts',(1.86195461813654,0.816666666666665,-1.075));
#18432=CARTESIAN_POINT('Ctrl Pts',(2.48260615751539,0.874999999999999,-7.60078921086183E-16));
#18433=CARTESIAN_POINT('Ctrl Pts',(1.86195461813654,0.933333333333332,1.075));
#18434=CARTESIAN_POINT('Ctrl Pts',(1.2413030787577,0.991666666666665,2.15));
#18435=CARTESIAN_POINT('Ctrl Pts',(7.89897185450043E-16,1.05,2.15));
#18436=CARTESIAN_POINT('Ctrl Pts',(-1.24130307875769,1.10833333333333,2.15));
#18437=CARTESIAN_POINT('Ctrl Pts',(-1.86195461813654,1.16666666666666,1.075));
#18438=CARTESIAN_POINT('Ctrl Pts',(-2.48260615751539,1.225,3.26910770324048E-15));
#18439=CARTESIAN_POINT('Ctrl Pts',(-1.86195461813654,1.28333333333333,-1.075));
#18440=CARTESIAN_POINT('Ctrl Pts',(-1.2413030787577,1.34166666666666,-2.15));
#18441=CARTESIAN_POINT('Ctrl Pts',(-1.05319624726672E-15,1.4,-2.15));
#18442=CARTESIAN_POINT('Ctrl Pts',(1.24130307875769,1.45833333333333,-2.15));
#18443=CARTESIAN_POINT('Ctrl Pts',(1.86195461813654,1.51666666666666,-1.075));
#18444=CARTESIAN_POINT('Ctrl Pts',(2.48260615751539,1.575,-1.36814205795513E-15));
#18445=CARTESIAN_POINT('Ctrl Pts',(1.86195461813654,1.63333333333333,1.075));
#18446=CARTESIAN_POINT('Ctrl Pts',(1.2413030787577,1.69166666666666,2.15));
#18447=CARTESIAN_POINT('Ctrl Pts',(1.3164953090834E-15,1.75,2.15));
#18448=CARTESIAN_POINT('Ctrl Pts',(-1.24130307875769,1.80833333333333,2.15));
#18449=CARTESIAN_POINT('Ctrl Pts',(-1.86195461813654,1.86666666666666,1.075));
#18450=CARTESIAN_POINT('Ctrl Pts',(-2.48260615751539,1.925,6.08216805382924E-15));
#18451=CARTESIAN_POINT('Ctrl Pts',(-1.86195461813654,1.98333333333333,-1.075));
#18452=CARTESIAN_POINT('Ctrl Pts',(-1.2413030787577,2.04166666666666,-2.15));
#18453=CARTESIAN_POINT('Ctrl Pts',(-5.39896157561062E-15,2.1,-2.15));
#18454=CARTESIAN_POINT('Ctrl Pts',(1.24130307875769,2.15833333333333,-2.15));
#18455=CARTESIAN_POINT('Ctrl Pts',(1.86195461813654,2.21666666666666,-1.075));
#18456=CARTESIAN_POINT('Ctrl Pts',(2.48260615751539,2.275,-6.38619962226372E-15));
#18457=CARTESIAN_POINT('Ctrl Pts',(1.86195461813655,2.33333333333333,1.07499999999999));
#18458=CARTESIAN_POINT('Ctrl Pts',(1.2413030787577,2.39166666666666,2.15));
#18459=CARTESIAN_POINT('Ctrl Pts',(1.84309343271677E-15,2.45,2.15));
#18460=CARTESIAN_POINT('Ctrl Pts',(-1.24130307875769,2.50833333333333,2.15));
#18461=CARTESIAN_POINT('Ctrl Pts',(-1.86195461813654,2.56666666666666,1.075));
#18462=CARTESIAN_POINT('Ctrl Pts',(-2.48260615751539,2.62499999999999,6.69023119069819E-15));
#18463=CARTESIAN_POINT('Ctrl Pts',(-1.86195461813655,2.68333333333333,-1.07499999999999));
#18464=CARTESIAN_POINT('Ctrl Pts',(-1.2413030787577,2.74166666666666,-2.14999999999999));
#18465=CARTESIAN_POINT('Ctrl Pts',(-2.10639249453345E-15,2.79999999999999,
-2.15));
#18466=CARTESIAN_POINT('Ctrl Pts',(1.24130307875769,2.85833333333333,-2.15));
#18467=CARTESIAN_POINT('Ctrl Pts',(1.86195461813654,2.91666666666666,-1.075));
#18468=CARTESIAN_POINT('Ctrl Pts',(2.48260615751539,2.97499999999999,-6.99426275913266E-15));
#18469=CARTESIAN_POINT('Ctrl Pts',(1.86195461813655,3.03333333333333,1.07499999999999));
#18470=CARTESIAN_POINT('Ctrl Pts',(1.2413030787577,3.09166666666666,2.14999999999999));
#18471=CARTESIAN_POINT('Ctrl Pts',(2.36969155635013E-15,3.14999999999999,
2.15));
#18472=CARTESIAN_POINT('Ctrl Pts',(-1.24130307875769,3.20833333333333,2.15));
#18473=CARTESIAN_POINT('Ctrl Pts',(-1.86195461813654,3.26666666666666,1.075));
#18474=CARTESIAN_POINT('Ctrl Pts',(-2.48260615751539,3.32499999999999,7.29829432756713E-15));
#18475=CARTESIAN_POINT('Ctrl Pts',(-1.86195461813655,3.38333333333333,-1.07499999999999));
#18476=CARTESIAN_POINT('Ctrl Pts',(-1.2413030787577,3.44166666666666,-2.14999999999999));
#18477=CARTESIAN_POINT('Ctrl Pts',(-1.02713250275879E-14,3.49999999999999,
-2.15));
#18478=CARTESIAN_POINT('Ctrl Pts',(1.24130307875769,3.55833333333333,-2.15));
#18479=CARTESIAN_POINT('Ctrl Pts',(1.86195461813654,3.61666666666666,-1.075));
#18480=CARTESIAN_POINT('Ctrl Pts',(2.48260615751539,3.67499999999999,-7.60232589600161E-15));
#18481=CARTESIAN_POINT('Ctrl Pts',(1.86195461813655,3.73333333333333,1.07499999999999));
#18482=CARTESIAN_POINT('Ctrl Pts',(1.2413030787577,3.79166666666666,2.14999999999999));
#18483=CARTESIAN_POINT('Ctrl Pts',(1.05346240894046E-14,3.84999999999999,
2.15));
#18484=CARTESIAN_POINT('',(0.,0.,1.8));
#18485=CARTESIAN_POINT('Origin',(0.,0.,2.15));
#18486=CARTESIAN_POINT('Ctrl Pts',(0.,0.,1.8));
#18487=CARTESIAN_POINT('Ctrl Pts',(-1.03923048454133,0.0583333333333332,
1.8));
#18488=CARTESIAN_POINT('Ctrl Pts',(-1.55884572681199,0.116666666666666,
0.9));
#18489=CARTESIAN_POINT('Ctrl Pts',(-2.07846096908265,0.175,1.27269028646989E-16));
#18490=CARTESIAN_POINT('Ctrl Pts',(-1.55884572681199,0.233333333333333,
-0.9));
#18491=CARTESIAN_POINT('Ctrl Pts',(-1.03923048454133,0.291666666666666,
-1.8));
#18492=CARTESIAN_POINT('Ctrl Pts',(-2.20436423846524E-16,0.349999999999999,
-1.8));
#18493=CARTESIAN_POINT('Ctrl Pts',(1.03923048454133,0.408333333333333,-1.8));
#18494=CARTESIAN_POINT('Ctrl Pts',(1.55884572681199,0.466666666666666,-0.900000000000001));
#18495=CARTESIAN_POINT('Ctrl Pts',(2.07846096908265,0.524999999999999,-3.81807085940967E-16));
#18496=CARTESIAN_POINT('Ctrl Pts',(1.55884572681199,0.583333333333332,0.899999999999999));
#18497=CARTESIAN_POINT('Ctrl Pts',(1.03923048454133,0.641666666666665,1.8));
#18498=CARTESIAN_POINT('Ctrl Pts',(4.40872847693047E-16,0.699999999999999,
1.8));
#18499=CARTESIAN_POINT('Ctrl Pts',(-1.03923048454132,0.758333333333332,
1.8));
#18500=CARTESIAN_POINT('Ctrl Pts',(-1.55884572681199,0.816666666666665,
0.900000000000001));
#18501=CARTESIAN_POINT('Ctrl Pts',(-2.07846096908265,0.874999999999998,
2.48238932216317E-15));
#18502=CARTESIAN_POINT('Ctrl Pts',(-1.55884572681199,0.933333333333332,
-0.899999999999999));
#18503=CARTESIAN_POINT('Ctrl Pts',(-1.03923048454133,0.991666666666665,
-1.8));
#18504=CARTESIAN_POINT('Ctrl Pts',(-6.61309271539571E-16,1.05,-1.8));
#18505=CARTESIAN_POINT('Ctrl Pts',(1.03923048454132,1.10833333333333,-1.8));
#18506=CARTESIAN_POINT('Ctrl Pts',(1.55884572681199,1.16666666666666,-0.900000000000002));
#18507=CARTESIAN_POINT('Ctrl Pts',(2.07846096908265,1.225,-8.90883200528922E-16));
#18508=CARTESIAN_POINT('Ctrl Pts',(1.55884572681199,1.28333333333333,0.899999999999998));
#18509=CARTESIAN_POINT('Ctrl Pts',(1.03923048454133,1.34166666666666,1.8));
#18510=CARTESIAN_POINT('Ctrl Pts',(8.81745695386094E-16,1.4,1.8));
#18511=CARTESIAN_POINT('Ctrl Pts',(-1.03923048454132,1.45833333333333,1.8));
#18512=CARTESIAN_POINT('Ctrl Pts',(-1.55884572681199,1.51666666666666,0.900000000000003));
#18513=CARTESIAN_POINT('Ctrl Pts',(-2.07846096908265,1.575,4.83750961567934E-15));
#18514=CARTESIAN_POINT('Ctrl Pts',(-1.55884572681199,1.63333333333333,-0.899999999999998));
#18515=CARTESIAN_POINT('Ctrl Pts',(-1.03923048454133,1.69166666666666,-1.8));
#18516=CARTESIAN_POINT('Ctrl Pts',(-4.29962443015307E-15,1.75,-1.8));
#18517=CARTESIAN_POINT('Ctrl Pts',(1.03923048454132,1.80833333333333,-1.8));
#18518=CARTESIAN_POINT('Ctrl Pts',(1.55884572681199,1.86666666666666,-0.900000000000003));
#18519=CARTESIAN_POINT('Ctrl Pts',(2.07846096908265,1.925,-5.09204767297332E-15));
#18520=CARTESIAN_POINT('Ctrl Pts',(1.55884572681199,1.98333333333333,0.899999999999995));
#18521=CARTESIAN_POINT('Ctrl Pts',(1.03923048454133,2.04166666666666,1.8));
#18522=CARTESIAN_POINT('Ctrl Pts',(1.32261854307914E-15,2.1,1.8));
#18523=CARTESIAN_POINT('Ctrl Pts',(-1.03923048454132,2.15833333333333,1.8));
#18524=CARTESIAN_POINT('Ctrl Pts',(-1.55884572681199,2.21666666666666,0.900000000000003));
#18525=CARTESIAN_POINT('Ctrl Pts',(-2.07846096908265,2.275,5.3465857302673E-15));
#18526=CARTESIAN_POINT('Ctrl Pts',(-1.55884572681199,2.33333333333333,-0.899999999999995));
#18527=CARTESIAN_POINT('Ctrl Pts',(-1.03923048454133,2.39166666666666,-1.8));
#18528=CARTESIAN_POINT('Ctrl Pts',(-1.54305496692567E-15,2.45,-1.8));
#18529=CARTESIAN_POINT('Ctrl Pts',(1.03923048454132,2.50833333333333,-1.8));
#18530=CARTESIAN_POINT('Ctrl Pts',(1.55884572681199,2.56666666666666,-0.900000000000003));
#18531=CARTESIAN_POINT('Ctrl Pts',(2.07846096908265,2.625,-5.60112378756128E-15));
#18532=CARTESIAN_POINT('Ctrl Pts',(1.55884572681199,2.68333333333333,0.899999999999995));
#18533=CARTESIAN_POINT('Ctrl Pts',(1.03923048454133,2.74166666666666,1.8));
#18534=CARTESIAN_POINT('Ctrl Pts',(1.76349139077219E-15,2.79999999999999,
1.8));
#18535=CARTESIAN_POINT('Ctrl Pts',(-1.03923048454132,2.85833333333333,1.8));
#18536=CARTESIAN_POINT('Ctrl Pts',(-1.55884572681199,2.91666666666666,0.900000000000003));
#18537=CARTESIAN_POINT('Ctrl Pts',(-2.07846096908265,2.97499999999999,5.85566184485525E-15));
#18538=CARTESIAN_POINT('Ctrl Pts',(-1.55884572681199,3.03333333333333,-0.899999999999995));
#18539=CARTESIAN_POINT('Ctrl Pts',(-1.03923048454133,3.09166666666666,-1.8));
#18540=CARTESIAN_POINT('Ctrl Pts',(-8.37881243645961E-15,3.14999999999999,
-1.8));
#18541=CARTESIAN_POINT('Ctrl Pts',(1.03923048454132,3.20833333333333,-1.8));
#18542=CARTESIAN_POINT('Ctrl Pts',(1.55884572681199,3.26666666666666,-0.900000000000004));
#18543=CARTESIAN_POINT('Ctrl Pts',(2.07846096908265,3.32499999999999,-6.11019990214923E-15));
#18544=CARTESIAN_POINT('Ctrl Pts',(1.55884572681199,3.38333333333333,0.899999999999995));
#18545=CARTESIAN_POINT('Ctrl Pts',(1.03923048454133,3.44166666666666,1.8));
#18546=CARTESIAN_POINT('Ctrl Pts',(8.59924886030614E-15,3.49999999999999,
1.8));
#18547=CARTESIAN_POINT('Ctrl Pts',(-1.03923048454132,3.55833333333333,1.8));
#18548=CARTESIAN_POINT('Ctrl Pts',(-1.55884572681199,3.61666666666666,0.900000000000004));
#18549=CARTESIAN_POINT('Ctrl Pts',(-2.07846096908265,3.67499999999999,1.37489146751561E-14));
#18550=CARTESIAN_POINT('Ctrl Pts',(-1.55884572681199,3.73333333333333,-0.899999999999994));
#18551=CARTESIAN_POINT('Ctrl Pts',(-1.03923048454133,3.79166666666666,-1.8));
#18552=CARTESIAN_POINT('Ctrl Pts',(-8.81968528415266E-15,3.84999999999999,
-1.8));
#18553=CARTESIAN_POINT('Ctrl Pts',(1.03923048454132,3.90833333333333,-1.8));
#18554=CARTESIAN_POINT('Ctrl Pts',(1.55884572681198,3.96666666666666,-0.90000000000001));
#18555=CARTESIAN_POINT('Ctrl Pts',(2.07846096908265,4.02499999999999,-6.61927601673719E-15));
#18556=CARTESIAN_POINT('Ctrl Pts',(1.558845726812,4.08333333333333,0.899999999999989));
#18557=CARTESIAN_POINT('Ctrl Pts',(1.03923048454133,4.14166666666666,1.8));
#18558=CARTESIAN_POINT('Ctrl Pts',(-7.40933783759325E-14,4.2,1.8));
#18559=CARTESIAN_POINT('Ctrl Pts',(0.,-0.35,2.15));
#18560=CARTESIAN_POINT('Ctrl Pts',(-1.2413030787577,-0.291666666666667,
2.15));
#18561=CARTESIAN_POINT('Ctrl Pts',(-1.86195461813654,-0.233333333333334,
1.075));
#18562=CARTESIAN_POINT('Ctrl Pts',(-2.48260615751539,-0.175,1.52015784217237E-16));
#18563=CARTESIAN_POINT('Ctrl Pts',(-1.86195461813654,-0.116666666666667,
-1.075));
#18564=CARTESIAN_POINT('Ctrl Pts',(-1.2413030787577,-0.058333333333334,
-2.15));
#18565=CARTESIAN_POINT('Ctrl Pts',(-2.63299061816681E-16,-7.58941520739853E-16,
-2.15));
#18566=CARTESIAN_POINT('Ctrl Pts',(1.24130307875769,0.0583333333333325,
-2.15));
#18567=CARTESIAN_POINT('Ctrl Pts',(1.86195461813654,0.116666666666666,-1.075));
#18568=CARTESIAN_POINT('Ctrl Pts',(2.48260615751539,0.174999999999999,-4.5604735265171E-16));
#18569=CARTESIAN_POINT('Ctrl Pts',(1.86195461813654,0.233333333333332,1.075));
#18570=CARTESIAN_POINT('Ctrl Pts',(1.2413030787577,0.291666666666665,2.15));
#18571=CARTESIAN_POINT('Ctrl Pts',(0.,0.349999999999999,2.15));
#18572=CARTESIAN_POINT('Ctrl Pts',(-1.2413030787577,0.408333333333332,2.15));
#18573=CARTESIAN_POINT('Ctrl Pts',(-1.86195461813654,0.466666666666665,
1.075));
#18574=CARTESIAN_POINT('Ctrl Pts',(-2.48260615751539,0.524999999999998,
1.52015784217237E-16));
#18575=CARTESIAN_POINT('Ctrl Pts',(-1.86195461813654,0.583333333333331,
-1.075));
#18576=CARTESIAN_POINT('Ctrl Pts',(-1.2413030787577,0.641666666666665,-2.15));
#18577=CARTESIAN_POINT('Ctrl Pts',(-2.63299061816681E-16,0.699999999999998,
-2.15));
#18578=CARTESIAN_POINT('Ctrl Pts',(1.24130307875769,0.758333333333331,-2.15));
#18579=CARTESIAN_POINT('Ctrl Pts',(1.86195461813654,0.816666666666664,-1.075));
#18580=CARTESIAN_POINT('Ctrl Pts',(2.48260615751539,0.874999999999997,-4.5604735265171E-16));
#18581=CARTESIAN_POINT('Ctrl Pts',(1.86195461813654,0.933333333333331,1.075));
#18582=CARTESIAN_POINT('Ctrl Pts',(1.2413030787577,0.991666666666664,2.15));
#18583=CARTESIAN_POINT('Ctrl Pts',(0.,1.05,2.15));
#18584=CARTESIAN_POINT('Ctrl Pts',(-1.2413030787577,1.10833333333333,2.15));
#18585=CARTESIAN_POINT('Ctrl Pts',(-1.86195461813654,1.16666666666666,1.075));
#18586=CARTESIAN_POINT('Ctrl Pts',(-2.48260615751539,1.225,1.52015784217237E-16));
#18587=CARTESIAN_POINT('Ctrl Pts',(-1.86195461813654,1.28333333333333,-1.075));
#18588=CARTESIAN_POINT('Ctrl Pts',(-1.2413030787577,1.34166666666666,-2.15));
#18589=CARTESIAN_POINT('Ctrl Pts',(-2.63299061816681E-16,1.4,-2.15));
#18590=CARTESIAN_POINT('Ctrl Pts',(1.24130307875769,1.45833333333333,-2.15));
#18591=CARTESIAN_POINT('Ctrl Pts',(1.86195461813654,1.51666666666666,-1.075));
#18592=CARTESIAN_POINT('Ctrl Pts',(2.48260615751539,1.575,-4.5604735265171E-16));
#18593=CARTESIAN_POINT('Ctrl Pts',(1.86195461813654,1.63333333333333,1.075));
#18594=CARTESIAN_POINT('Ctrl Pts',(1.2413030787577,1.69166666666666,2.15));
#18595=CARTESIAN_POINT('Ctrl Pts',(0.,1.75,2.15));
#18596=CARTESIAN_POINT('Ctrl Pts',(-1.2413030787577,1.80833333333333,2.15));
#18597=CARTESIAN_POINT('Ctrl Pts',(-1.86195461813654,1.86666666666666,1.075));
#18598=CARTESIAN_POINT('Ctrl Pts',(-2.48260615751539,1.925,1.52015784217237E-16));
#18599=CARTESIAN_POINT('Ctrl Pts',(-1.86195461813654,1.98333333333333,-1.075));
#18600=CARTESIAN_POINT('Ctrl Pts',(-1.2413030787577,2.04166666666666,-2.15));
#18601=CARTESIAN_POINT('Ctrl Pts',(-2.63299061816681E-16,2.1,-2.15));
#18602=CARTESIAN_POINT('Ctrl Pts',(1.24130307875769,2.15833333333333,-2.15));
#18603=CARTESIAN_POINT('Ctrl Pts',(1.86195461813654,2.21666666666666,-1.075));
#18604=CARTESIAN_POINT('Ctrl Pts',(2.48260615751539,2.275,-4.5604735265171E-16));
#18605=CARTESIAN_POINT('Ctrl Pts',(1.86195461813654,2.33333333333333,1.075));
#18606=CARTESIAN_POINT('Ctrl Pts',(1.2413030787577,2.39166666666666,2.15));
#18607=CARTESIAN_POINT('Ctrl Pts',(0.,2.44999999999999,2.15));
#18608=CARTESIAN_POINT('Ctrl Pts',(-1.2413030787577,2.50833333333333,2.15));
#18609=CARTESIAN_POINT('Ctrl Pts',(-1.86195461813654,2.56666666666666,1.075));
#18610=CARTESIAN_POINT('Ctrl Pts',(-2.48260615751539,2.62499999999999,1.52015784217237E-16));
#18611=CARTESIAN_POINT('Ctrl Pts',(-1.86195461813654,2.68333333333333,-1.075));
#18612=CARTESIAN_POINT('Ctrl Pts',(-1.2413030787577,2.74166666666666,-2.15));
#18613=CARTESIAN_POINT('Ctrl Pts',(-2.63299061816681E-16,2.79999999999999,
-2.15));
#18614=CARTESIAN_POINT('Ctrl Pts',(1.24130307875769,2.85833333333333,-2.15));
#18615=CARTESIAN_POINT('Ctrl Pts',(1.86195461813654,2.91666666666666,-1.075));
#18616=CARTESIAN_POINT('Ctrl Pts',(2.48260615751539,2.97499999999999,-4.5604735265171E-16));
#18617=CARTESIAN_POINT('Ctrl Pts',(1.86195461813654,3.03333333333333,1.075));
#18618=CARTESIAN_POINT('Ctrl Pts',(1.2413030787577,3.09166666666666,2.15));
#18619=CARTESIAN_POINT('Ctrl Pts',(0.,3.14999999999999,2.15));
#18620=CARTESIAN_POINT('Ctrl Pts',(-1.2413030787577,3.20833333333333,2.15));
#18621=CARTESIAN_POINT('Ctrl Pts',(-1.86195461813654,3.26666666666666,1.075));
#18622=CARTESIAN_POINT('Ctrl Pts',(-2.48260615751539,3.32499999999999,1.52015784217237E-16));
#18623=CARTESIAN_POINT('Ctrl Pts',(-1.86195461813654,3.38333333333333,-1.075));
#18624=CARTESIAN_POINT('Ctrl Pts',(-1.2413030787577,3.44166666666666,-2.15));
#18625=CARTESIAN_POINT('Ctrl Pts',(-2.63299061816681E-16,3.49999999999999,
-2.15));
#18626=CARTESIAN_POINT('Ctrl Pts',(1.24130307875769,3.55833333333333,-2.15));
#18627=CARTESIAN_POINT('Ctrl Pts',(1.86195461813654,3.61666666666666,-1.075));
#18628=CARTESIAN_POINT('Ctrl Pts',(2.48260615751539,3.67499999999999,-4.5604735265171E-16));
#18629=CARTESIAN_POINT('Ctrl Pts',(1.86195461813654,3.73333333333333,1.075));
#18630=CARTESIAN_POINT('Ctrl Pts',(1.2413030787577,3.79166666666666,2.15));
#18631=CARTESIAN_POINT('Ctrl Pts',(0.,3.84999999999999,2.15));
#18632=CARTESIAN_POINT('Ctrl Pts',(0.,-0.35,1.94497474683058));
#18633=CARTESIAN_POINT('Ctrl Pts',(-1.12293169364966,-0.291666666666667,
1.94497474683058));
#18634=CARTESIAN_POINT('Ctrl Pts',(-1.68439754047449,-0.233333333333334,
0.972487373415292));
#18635=CARTESIAN_POINT('Ctrl Pts',(-2.24586338729932,-0.175,1.37519470428917E-16));
#18636=CARTESIAN_POINT('Ctrl Pts',(-1.68439754047449,-0.116666666666667,
-0.972487373415291));
#18637=CARTESIAN_POINT('Ctrl Pts',(-1.12293169364966,-0.058333333333334,
-1.94497474683058));
#18638=CARTESIAN_POINT('Ctrl Pts',(-2.38190709812851E-16,-8.13151629364128E-16,
-1.94497474683058));
#18639=CARTESIAN_POINT('Ctrl Pts',(1.12293169364966,0.0583333333333324,
-1.94497474683058));
#18640=CARTESIAN_POINT('Ctrl Pts',(1.68439754047449,0.116666666666666,-0.972487373415292));
#18641=CARTESIAN_POINT('Ctrl Pts',(2.24586338729932,0.174999999999999,-4.12558411286752E-16));
#18642=CARTESIAN_POINT('Ctrl Pts',(1.68439754047449,0.233333333333332,0.97248737341529));
#18643=CARTESIAN_POINT('Ctrl Pts',(1.12293169364966,0.291666666666665,1.94497474683058));
#18644=CARTESIAN_POINT('Ctrl Pts',(0.,0.349999999999998,1.94497474683058));
#18645=CARTESIAN_POINT('Ctrl Pts',(-1.12293169364966,0.408333333333332,
1.94497474683058));
#18646=CARTESIAN_POINT('Ctrl Pts',(-1.68439754047449,0.466666666666665,
0.972487373415292));
#18647=CARTESIAN_POINT('Ctrl Pts',(-2.24586338729932,0.524999999999998,
1.37519470428917E-16));
#18648=CARTESIAN_POINT('Ctrl Pts',(-1.68439754047449,0.583333333333331,
-0.972487373415291));
#18649=CARTESIAN_POINT('Ctrl Pts',(-1.12293169364966,0.641666666666665,
-1.94497474683058));
#18650=CARTESIAN_POINT('Ctrl Pts',(-2.38190709812851E-16,0.699999999999998,
-1.94497474683058));
#18651=CARTESIAN_POINT('Ctrl Pts',(1.12293169364966,0.758333333333331,-1.94497474683058));
#18652=CARTESIAN_POINT('Ctrl Pts',(1.68439754047449,0.816666666666664,-0.972487373415292));
#18653=CARTESIAN_POINT('Ctrl Pts',(2.24586338729932,0.874999999999998,-4.12558411286752E-16));
#18654=CARTESIAN_POINT('Ctrl Pts',(1.68439754047449,0.933333333333331,0.97248737341529));
#18655=CARTESIAN_POINT('Ctrl Pts',(1.12293169364966,0.991666666666664,1.94497474683058));
#18656=CARTESIAN_POINT('Ctrl Pts',(0.,1.05,1.94497474683058));
#18657=CARTESIAN_POINT('Ctrl Pts',(-1.12293169364966,1.10833333333333,1.94497474683058));
#18658=CARTESIAN_POINT('Ctrl Pts',(-1.68439754047449,1.16666666666666,0.972487373415292));
#18659=CARTESIAN_POINT('Ctrl Pts',(-2.24586338729932,1.225,1.37519470428917E-16));
#18660=CARTESIAN_POINT('Ctrl Pts',(-1.68439754047449,1.28333333333333,-0.972487373415291));
#18661=CARTESIAN_POINT('Ctrl Pts',(-1.12293169364966,1.34166666666666,-1.94497474683058));
#18662=CARTESIAN_POINT('Ctrl Pts',(-2.38190709812851E-16,1.4,-1.94497474683058));
#18663=CARTESIAN_POINT('Ctrl Pts',(1.12293169364966,1.45833333333333,-1.94497474683058));
#18664=CARTESIAN_POINT('Ctrl Pts',(1.68439754047449,1.51666666666666,-0.972487373415292));
#18665=CARTESIAN_POINT('Ctrl Pts',(2.24586338729932,1.575,-4.12558411286752E-16));
#18666=CARTESIAN_POINT('Ctrl Pts',(1.68439754047449,1.63333333333333,0.97248737341529));
#18667=CARTESIAN_POINT('Ctrl Pts',(1.12293169364966,1.69166666666666,1.94497474683058));
#18668=CARTESIAN_POINT('Ctrl Pts',(0.,1.75,1.94497474683058));
#18669=CARTESIAN_POINT('Ctrl Pts',(-1.12293169364966,1.80833333333333,1.94497474683058));
#18670=CARTESIAN_POINT('Ctrl Pts',(-1.68439754047449,1.86666666666666,0.972487373415292));
#18671=CARTESIAN_POINT('Ctrl Pts',(-2.24586338729932,1.925,1.37519470428917E-16));
#18672=CARTESIAN_POINT('Ctrl Pts',(-1.68439754047449,1.98333333333333,-0.972487373415291));
#18673=CARTESIAN_POINT('Ctrl Pts',(-1.12293169364966,2.04166666666666,-1.94497474683058));
#18674=CARTESIAN_POINT('Ctrl Pts',(-2.38190709812851E-16,2.09999999999999,
-1.94497474683058));
#18675=CARTESIAN_POINT('Ctrl Pts',(1.12293169364966,2.15833333333333,-1.94497474683058));
#18676=CARTESIAN_POINT('Ctrl Pts',(1.68439754047449,2.21666666666666,-0.972487373415292));
#18677=CARTESIAN_POINT('Ctrl Pts',(2.24586338729932,2.275,-4.12558411286752E-16));
#18678=CARTESIAN_POINT('Ctrl Pts',(1.68439754047449,2.33333333333333,0.97248737341529));
#18679=CARTESIAN_POINT('Ctrl Pts',(1.12293169364966,2.39166666666666,1.94497474683058));
#18680=CARTESIAN_POINT('Ctrl Pts',(0.,2.44999999999999,1.94497474683058));
#18681=CARTESIAN_POINT('Ctrl Pts',(-1.12293169364966,2.50833333333333,1.94497474683058));
#18682=CARTESIAN_POINT('Ctrl Pts',(-1.68439754047449,2.56666666666666,0.972487373415292));
#18683=CARTESIAN_POINT('Ctrl Pts',(-2.24586338729932,2.62499999999999,1.37519470428917E-16));
#18684=CARTESIAN_POINT('Ctrl Pts',(-1.68439754047449,2.68333333333333,-0.972487373415291));
#18685=CARTESIAN_POINT('Ctrl Pts',(-1.12293169364966,2.74166666666666,-1.94497474683058));
#18686=CARTESIAN_POINT('Ctrl Pts',(-2.38190709812851E-16,2.79999999999999,
-1.94497474683058));
#18687=CARTESIAN_POINT('Ctrl Pts',(1.12293169364966,2.85833333333333,-1.94497474683058));
#18688=CARTESIAN_POINT('Ctrl Pts',(1.68439754047449,2.91666666666666,-0.972487373415292));
#18689=CARTESIAN_POINT('Ctrl Pts',(2.24586338729932,2.97499999999999,-4.12558411286752E-16));
#18690=CARTESIAN_POINT('Ctrl Pts',(1.68439754047449,3.03333333333333,0.97248737341529));
#18691=CARTESIAN_POINT('Ctrl Pts',(1.12293169364966,3.09166666666666,1.94497474683058));
#18692=CARTESIAN_POINT('Ctrl Pts',(0.,3.14999999999999,1.94497474683058));
#18693=CARTESIAN_POINT('Ctrl Pts',(-1.12293169364966,3.20833333333333,1.94497474683058));
#18694=CARTESIAN_POINT('Ctrl Pts',(-1.68439754047449,3.26666666666666,0.972487373415292));
#18695=CARTESIAN_POINT('Ctrl Pts',(-2.24586338729932,3.32499999999999,1.37519470428917E-16));
#18696=CARTESIAN_POINT('Ctrl Pts',(-1.68439754047449,3.38333333333333,-0.972487373415291));
#18697=CARTESIAN_POINT('Ctrl Pts',(-1.12293169364966,3.44166666666666,-1.94497474683058));
#18698=CARTESIAN_POINT('Ctrl Pts',(-2.38190709812851E-16,3.49999999999999,
-1.94497474683058));
#18699=CARTESIAN_POINT('Ctrl Pts',(1.12293169364966,3.55833333333333,-1.94497474683058));
#18700=CARTESIAN_POINT('Ctrl Pts',(1.68439754047449,3.61666666666666,-0.972487373415292));
#18701=CARTESIAN_POINT('Ctrl Pts',(2.24586338729932,3.67499999999999,-4.12558411286752E-16));
#18702=CARTESIAN_POINT('Ctrl Pts',(1.68439754047449,3.73333333333332,0.97248737341529));
#18703=CARTESIAN_POINT('Ctrl Pts',(1.12293169364966,3.79166666666666,1.94497474683058));
#18704=CARTESIAN_POINT('Ctrl Pts',(0.,3.84999999999999,1.94497474683058));
#18705=CARTESIAN_POINT('Ctrl Pts',(0.,-0.205025253169417,1.8));
#18706=CARTESIAN_POINT('Ctrl Pts',(-1.03923048454133,-0.146691919836083,
1.8));
#18707=CARTESIAN_POINT('Ctrl Pts',(-1.55884572681199,-0.0883585865027503,
0.9));
#18708=CARTESIAN_POINT('Ctrl Pts',(-2.07846096908265,-0.0300252531694171,
1.27269028646989E-16));
#18709=CARTESIAN_POINT('Ctrl Pts',(-1.55884572681199,0.0283080801639161,
-0.9));
#18710=CARTESIAN_POINT('Ctrl Pts',(-1.03923048454133,0.0866414134972494,
-1.8));
#18711=CARTESIAN_POINT('Ctrl Pts',(-2.20436423846524E-16,0.144974746830583,
-1.8));
#18712=CARTESIAN_POINT('Ctrl Pts',(1.03923048454133,0.203308080163916,-1.8));
#18713=CARTESIAN_POINT('Ctrl Pts',(1.55884572681199,0.261641413497249,-0.900000000000001));
#18714=CARTESIAN_POINT('Ctrl Pts',(2.07846096908265,0.319974746830582,-3.81807085940967E-16));
#18715=CARTESIAN_POINT('Ctrl Pts',(1.55884572681199,0.378308080163915,0.899999999999999));
#18716=CARTESIAN_POINT('Ctrl Pts',(1.03923048454133,0.436641413497249,1.8));
#18717=CARTESIAN_POINT('Ctrl Pts',(0.,0.494974746830582,1.8));
#18718=CARTESIAN_POINT('Ctrl Pts',(-1.03923048454133,0.553308080163915,
1.8));
#18719=CARTESIAN_POINT('Ctrl Pts',(-1.55884572681199,0.611641413497248,
0.9));
#18720=CARTESIAN_POINT('Ctrl Pts',(-2.07846096908265,0.669974746830582,
1.27269028646989E-16));
#18721=CARTESIAN_POINT('Ctrl Pts',(-1.55884572681199,0.728308080163915,
-0.9));
#18722=CARTESIAN_POINT('Ctrl Pts',(-1.03923048454133,0.786641413497248,
-1.8));
#18723=CARTESIAN_POINT('Ctrl Pts',(-2.20436423846524E-16,0.844974746830581,
-1.8));
#18724=CARTESIAN_POINT('Ctrl Pts',(1.03923048454133,0.903308080163914,-1.8));
#18725=CARTESIAN_POINT('Ctrl Pts',(1.55884572681199,0.961641413497248,-0.900000000000001));
#18726=CARTESIAN_POINT('Ctrl Pts',(2.07846096908265,1.01997474683058,-3.81807085940967E-16));
#18727=CARTESIAN_POINT('Ctrl Pts',(1.55884572681199,1.07830808016391,0.899999999999999));
#18728=CARTESIAN_POINT('Ctrl Pts',(1.03923048454133,1.13664141349725,1.8));
#18729=CARTESIAN_POINT('Ctrl Pts',(0.,1.19497474683058,1.8));
#18730=CARTESIAN_POINT('Ctrl Pts',(-1.03923048454133,1.25330808016391,1.8));
#18731=CARTESIAN_POINT('Ctrl Pts',(-1.55884572681199,1.31164141349725,0.9));
#18732=CARTESIAN_POINT('Ctrl Pts',(-2.07846096908265,1.36997474683058,1.27269028646989E-16));
#18733=CARTESIAN_POINT('Ctrl Pts',(-1.55884572681199,1.42830808016391,-0.9));
#18734=CARTESIAN_POINT('Ctrl Pts',(-1.03923048454133,1.48664141349725,-1.8));
#18735=CARTESIAN_POINT('Ctrl Pts',(-2.20436423846524E-16,1.54497474683058,
-1.8));
#18736=CARTESIAN_POINT('Ctrl Pts',(1.03923048454133,1.60330808016391,-1.8));
#18737=CARTESIAN_POINT('Ctrl Pts',(1.55884572681199,1.66164141349725,-0.900000000000001));
#18738=CARTESIAN_POINT('Ctrl Pts',(2.07846096908265,1.71997474683058,-3.81807085940967E-16));
#18739=CARTESIAN_POINT('Ctrl Pts',(1.55884572681199,1.77830808016391,0.899999999999999));
#18740=CARTESIAN_POINT('Ctrl Pts',(1.03923048454133,1.83664141349725,1.8));
#18741=CARTESIAN_POINT('Ctrl Pts',(0.,1.89497474683058,1.8));
#18742=CARTESIAN_POINT('Ctrl Pts',(-1.03923048454133,1.95330808016391,1.8));
#18743=CARTESIAN_POINT('Ctrl Pts',(-1.55884572681199,2.01164141349725,0.9));
#18744=CARTESIAN_POINT('Ctrl Pts',(-2.07846096908265,2.06997474683058,1.27269028646989E-16));
#18745=CARTESIAN_POINT('Ctrl Pts',(-1.55884572681199,2.12830808016391,-0.9));
#18746=CARTESIAN_POINT('Ctrl Pts',(-1.03923048454133,2.18664141349725,-1.8));
#18747=CARTESIAN_POINT('Ctrl Pts',(-2.20436423846524E-16,2.24497474683058,
-1.8));
#18748=CARTESIAN_POINT('Ctrl Pts',(1.03923048454133,2.30330808016391,-1.8));
#18749=CARTESIAN_POINT('Ctrl Pts',(1.55884572681199,2.36164141349724,-0.900000000000001));
#18750=CARTESIAN_POINT('Ctrl Pts',(2.07846096908265,2.41997474683058,-3.81807085940967E-16));
#18751=CARTESIAN_POINT('Ctrl Pts',(1.55884572681199,2.47830808016391,0.899999999999999));
#18752=CARTESIAN_POINT('Ctrl Pts',(1.03923048454133,2.53664141349724,1.8));
#18753=CARTESIAN_POINT('Ctrl Pts',(0.,2.59497474683058,1.8));
#18754=CARTESIAN_POINT('Ctrl Pts',(-1.03923048454133,2.65330808016391,1.8));
#18755=CARTESIAN_POINT('Ctrl Pts',(-1.55884572681199,2.71164141349724,0.9));
#18756=CARTESIAN_POINT('Ctrl Pts',(-2.07846096908265,2.76997474683058,1.27269028646989E-16));
#18757=CARTESIAN_POINT('Ctrl Pts',(-1.55884572681199,2.82830808016391,-0.9));
#18758=CARTESIAN_POINT('Ctrl Pts',(-1.03923048454133,2.88664141349724,-1.8));
#18759=CARTESIAN_POINT('Ctrl Pts',(-2.20436423846524E-16,2.94497474683058,
-1.8));
#18760=CARTESIAN_POINT('Ctrl Pts',(1.03923048454133,3.00330808016391,-1.8));
#18761=CARTESIAN_POINT('Ctrl Pts',(1.55884572681199,3.06164141349724,-0.900000000000001));
#18762=CARTESIAN_POINT('Ctrl Pts',(2.07846096908265,3.11997474683058,-3.81807085940967E-16));
#18763=CARTESIAN_POINT('Ctrl Pts',(1.55884572681199,3.17830808016391,0.899999999999999));
#18764=CARTESIAN_POINT('Ctrl Pts',(1.03923048454133,3.23664141349724,1.8));
#18765=CARTESIAN_POINT('Ctrl Pts',(0.,3.29497474683058,1.8));
#18766=CARTESIAN_POINT('Ctrl Pts',(-1.03923048454133,3.35330808016391,1.8));
#18767=CARTESIAN_POINT('Ctrl Pts',(-1.55884572681199,3.41164141349724,0.9));
#18768=CARTESIAN_POINT('Ctrl Pts',(-2.07846096908265,3.46997474683058,1.27269028646989E-16));
#18769=CARTESIAN_POINT('Ctrl Pts',(-1.55884572681199,3.52830808016391,-0.9));
#18770=CARTESIAN_POINT('Ctrl Pts',(-1.03923048454133,3.58664141349724,-1.8));
#18771=CARTESIAN_POINT('Ctrl Pts',(-2.20436423846524E-16,3.64497474683058,
-1.8));
#18772=CARTESIAN_POINT('Ctrl Pts',(1.03923048454133,3.70330808016391,-1.8));
#18773=CARTESIAN_POINT('Ctrl Pts',(1.55884572681199,3.76164141349724,-0.900000000000001));
#18774=CARTESIAN_POINT('Ctrl Pts',(2.07846096908265,3.81997474683058,-3.81807085940967E-16));
#18775=CARTESIAN_POINT('Ctrl Pts',(1.55884572681199,3.87830808016391,0.899999999999999));
#18776=CARTESIAN_POINT('Ctrl Pts',(1.03923048454133,3.93664141349724,1.8));
#18777=CARTESIAN_POINT('Ctrl Pts',(0.,3.99497474683058,1.8));
#18778=CARTESIAN_POINT('Ctrl Pts',(0.,0.,1.8));
#18779=CARTESIAN_POINT('Ctrl Pts',(-1.03923048454133,0.0583333333333332,
1.8));
#18780=CARTESIAN_POINT('Ctrl Pts',(-1.55884572681199,0.116666666666666,
0.9));
#18781=CARTESIAN_POINT('Ctrl Pts',(-2.07846096908265,0.175,1.27269028646989E-16));
#18782=CARTESIAN_POINT('Ctrl Pts',(-1.55884572681199,0.233333333333333,
-0.9));
#18783=CARTESIAN_POINT('Ctrl Pts',(-1.03923048454133,0.291666666666666,
-1.8));
#18784=CARTESIAN_POINT('Ctrl Pts',(-2.20436423846524E-16,0.349999999999999,
-1.8));
#18785=CARTESIAN_POINT('Ctrl Pts',(1.03923048454133,0.408333333333333,-1.8));
#18786=CARTESIAN_POINT('Ctrl Pts',(1.55884572681199,0.466666666666666,-0.900000000000001));
#18787=CARTESIAN_POINT('Ctrl Pts',(2.07846096908265,0.524999999999999,-3.81807085940967E-16));
#18788=CARTESIAN_POINT('Ctrl Pts',(1.55884572681199,0.583333333333332,0.899999999999999));
#18789=CARTESIAN_POINT('Ctrl Pts',(1.03923048454133,0.641666666666665,1.8));
#18790=CARTESIAN_POINT('Ctrl Pts',(0.,0.699999999999999,1.8));
#18791=CARTESIAN_POINT('Ctrl Pts',(-1.03923048454133,0.758333333333332,
1.8));
#18792=CARTESIAN_POINT('Ctrl Pts',(-1.55884572681199,0.816666666666665,
0.9));
#18793=CARTESIAN_POINT('Ctrl Pts',(-2.07846096908265,0.874999999999998,
1.27269028646989E-16));
#18794=CARTESIAN_POINT('Ctrl Pts',(-1.55884572681199,0.933333333333332,
-0.9));
#18795=CARTESIAN_POINT('Ctrl Pts',(-1.03923048454133,0.991666666666665,
-1.8));
#18796=CARTESIAN_POINT('Ctrl Pts',(-2.20436423846524E-16,1.05,-1.8));
#18797=CARTESIAN_POINT('Ctrl Pts',(1.03923048454133,1.10833333333333,-1.8));
#18798=CARTESIAN_POINT('Ctrl Pts',(1.55884572681199,1.16666666666666,-0.900000000000001));
#18799=CARTESIAN_POINT('Ctrl Pts',(2.07846096908265,1.225,-3.81807085940967E-16));
#18800=CARTESIAN_POINT('Ctrl Pts',(1.55884572681199,1.28333333333333,0.899999999999999));
#18801=CARTESIAN_POINT('Ctrl Pts',(1.03923048454133,1.34166666666666,1.8));
#18802=CARTESIAN_POINT('Ctrl Pts',(0.,1.4,1.8));
#18803=CARTESIAN_POINT('Ctrl Pts',(-1.03923048454133,1.45833333333333,1.8));
#18804=CARTESIAN_POINT('Ctrl Pts',(-1.55884572681199,1.51666666666666,0.9));
#18805=CARTESIAN_POINT('Ctrl Pts',(-2.07846096908265,1.575,1.27269028646989E-16));
#18806=CARTESIAN_POINT('Ctrl Pts',(-1.55884572681199,1.63333333333333,-0.9));
#18807=CARTESIAN_POINT('Ctrl Pts',(-1.03923048454133,1.69166666666666,-1.8));
#18808=CARTESIAN_POINT('Ctrl Pts',(-2.20436423846524E-16,1.75,-1.8));
#18809=CARTESIAN_POINT('Ctrl Pts',(1.03923048454133,1.80833333333333,-1.8));
#18810=CARTESIAN_POINT('Ctrl Pts',(1.55884572681199,1.86666666666666,-0.900000000000001));
#18811=CARTESIAN_POINT('Ctrl Pts',(2.07846096908265,1.925,-3.81807085940967E-16));
#18812=CARTESIAN_POINT('Ctrl Pts',(1.55884572681199,1.98333333333333,0.899999999999999));
#18813=CARTESIAN_POINT('Ctrl Pts',(1.03923048454133,2.04166666666666,1.8));
#18814=CARTESIAN_POINT('Ctrl Pts',(0.,2.1,1.8));
#18815=CARTESIAN_POINT('Ctrl Pts',(-1.03923048454133,2.15833333333333,1.8));
#18816=CARTESIAN_POINT('Ctrl Pts',(-1.55884572681199,2.21666666666666,0.9));
#18817=CARTESIAN_POINT('Ctrl Pts',(-2.07846096908265,2.275,1.27269028646989E-16));
#18818=CARTESIAN_POINT('Ctrl Pts',(-1.55884572681199,2.33333333333333,-0.9));
#18819=CARTESIAN_POINT('Ctrl Pts',(-1.03923048454133,2.39166666666666,-1.8));
#18820=CARTESIAN_POINT('Ctrl Pts',(-2.20436423846524E-16,2.45,-1.8));
#18821=CARTESIAN_POINT('Ctrl Pts',(1.03923048454133,2.50833333333333,-1.8));
#18822=CARTESIAN_POINT('Ctrl Pts',(1.55884572681199,2.56666666666666,-0.900000000000001));
#18823=CARTESIAN_POINT('Ctrl Pts',(2.07846096908265,2.62499999999999,-3.81807085940967E-16));
#18824=CARTESIAN_POINT('Ctrl Pts',(1.55884572681199,2.68333333333333,0.899999999999999));
#18825=CARTESIAN_POINT('Ctrl Pts',(1.03923048454133,2.74166666666666,1.8));
#18826=CARTESIAN_POINT('Ctrl Pts',(0.,2.79999999999999,1.8));
#18827=CARTESIAN_POINT('Ctrl Pts',(-1.03923048454133,2.85833333333333,1.8));
#18828=CARTESIAN_POINT('Ctrl Pts',(-1.55884572681199,2.91666666666666,0.9));
#18829=CARTESIAN_POINT('Ctrl Pts',(-2.07846096908265,2.97499999999999,1.27269028646989E-16));
#18830=CARTESIAN_POINT('Ctrl Pts',(-1.55884572681199,3.03333333333333,-0.9));
#18831=CARTESIAN_POINT('Ctrl Pts',(-1.03923048454133,3.09166666666666,-1.8));
#18832=CARTESIAN_POINT('Ctrl Pts',(-2.20436423846524E-16,3.14999999999999,
-1.8));
#18833=CARTESIAN_POINT('Ctrl Pts',(1.03923048454133,3.20833333333333,-1.8));
#18834=CARTESIAN_POINT('Ctrl Pts',(1.55884572681199,3.26666666666666,-0.900000000000001));
#18835=CARTESIAN_POINT('Ctrl Pts',(2.07846096908265,3.32499999999999,-3.81807085940967E-16));
#18836=CARTESIAN_POINT('Ctrl Pts',(1.55884572681199,3.38333333333333,0.899999999999999));
#18837=CARTESIAN_POINT('Ctrl Pts',(1.03923048454133,3.44166666666666,1.8));
#18838=CARTESIAN_POINT('Ctrl Pts',(0.,3.49999999999999,1.8));
#18839=CARTESIAN_POINT('Ctrl Pts',(-1.03923048454133,3.55833333333333,1.8));
#18840=CARTESIAN_POINT('Ctrl Pts',(-1.55884572681199,3.61666666666666,0.9));
#18841=CARTESIAN_POINT('Ctrl Pts',(-2.07846096908265,3.67499999999999,1.27269028646989E-16));
#18842=CARTESIAN_POINT('Ctrl Pts',(-1.55884572681199,3.73333333333333,-0.9));
#18843=CARTESIAN_POINT('Ctrl Pts',(-1.03923048454133,3.79166666666666,-1.8));
#18844=CARTESIAN_POINT('Ctrl Pts',(-2.20436423846524E-16,3.84999999999999,
-1.8));
#18845=CARTESIAN_POINT('Ctrl Pts',(1.03923048454133,3.90833333333333,-1.8));
#18846=CARTESIAN_POINT('Ctrl Pts',(1.55884572681199,3.96666666666666,-0.900000000000001));
#18847=CARTESIAN_POINT('Ctrl Pts',(2.07846096908265,4.02499999999999,-3.81807085940967E-16));
#18848=CARTESIAN_POINT('Ctrl Pts',(1.55884572681199,4.08333333333333,0.899999999999999));
#18849=CARTESIAN_POINT('Ctrl Pts',(1.03923048454133,4.14166666666666,1.8));
#18850=CARTESIAN_POINT('Ctrl Pts',(0.,4.19999999999999,1.8));
#18851=CARTESIAN_POINT('',(-2.63299061816681E-16,-0.349999999999999,2.15));
#18852=CARTESIAN_POINT('Origin',(0.,0.,2.15));
#18853=CARTESIAN_POINT('Ctrl Pts',(-2.63299061816681E-16,-0.349999999999999,
2.15));
#18854=CARTESIAN_POINT('Ctrl Pts',(-1.2413030787577,-0.291666666666666,
2.15));
#18855=CARTESIAN_POINT('Ctrl Pts',(-1.86195461813654,-0.233333333333333,
1.075));
#18856=CARTESIAN_POINT('Ctrl Pts',(-2.48260615751539,-0.175,-1.52015784217237E-16));
#18857=CARTESIAN_POINT('Ctrl Pts',(-1.86195461813654,-0.116666666666666,
-1.075));
#18858=CARTESIAN_POINT('Ctrl Pts',(-1.2413030787577,-0.0583333333333332,
-2.15));
#18859=CARTESIAN_POINT('Ctrl Pts',(0.,0.,-2.15));
#18860=CARTESIAN_POINT('Ctrl Pts',(1.24130307875769,0.0583333333333333,
-2.15));
#18861=CARTESIAN_POINT('Ctrl Pts',(1.86195461813654,0.116666666666666,-1.075));
#18862=CARTESIAN_POINT('Ctrl Pts',(2.48260615751539,0.175,-1.52015784217237E-16));
#18863=CARTESIAN_POINT('Ctrl Pts',(1.86195461813654,0.233333333333333,1.075));
#18864=CARTESIAN_POINT('Ctrl Pts',(1.2413030787577,0.291666666666666,2.15));
#18865=CARTESIAN_POINT('Ctrl Pts',(2.63299061816681E-16,0.349999999999999,
2.15));
#18866=CARTESIAN_POINT('Ctrl Pts',(2.63299061816681E-16,0.349999999999999,
2.15));
#18867=CARTESIAN_POINT('Ctrl Pts',(-1.24130307875769,0.408333333333333,
2.15));
#18868=CARTESIAN_POINT('Ctrl Pts',(-1.86195461813654,0.466666666666666,
1.075));
#18869=CARTESIAN_POINT('Ctrl Pts',(-2.48260615751539,0.524999999999999,
4.5604735265171E-16));
#18870=CARTESIAN_POINT('Ctrl Pts',(-1.86195461813654,0.583333333333332,
-1.075));
#18871=CARTESIAN_POINT('Ctrl Pts',(-1.2413030787577,0.641666666666665,-2.15));
#18872=CARTESIAN_POINT('Ctrl Pts',(-5.26598123633362E-16,0.699999999999999,
-2.15));
#18873=CARTESIAN_POINT('Ctrl Pts',(1.24130307875769,0.758333333333332,-2.15));
#18874=CARTESIAN_POINT('Ctrl Pts',(1.86195461813654,0.816666666666665,-1.075));
#18875=CARTESIAN_POINT('Ctrl Pts',(2.48260615751539,0.874999999999999,-7.60078921086183E-16));
#18876=CARTESIAN_POINT('Ctrl Pts',(1.86195461813654,0.933333333333332,1.075));
#18877=CARTESIAN_POINT('Ctrl Pts',(1.2413030787577,0.991666666666665,2.15));
#18878=CARTESIAN_POINT('Ctrl Pts',(7.89897185450043E-16,1.05,2.15));
#18879=CARTESIAN_POINT('Ctrl Pts',(-1.24130307875769,1.10833333333333,2.15));
#18880=CARTESIAN_POINT('Ctrl Pts',(-1.86195461813654,1.16666666666666,1.075));
#18881=CARTESIAN_POINT('Ctrl Pts',(-2.48260615751539,1.225,3.26910770324048E-15));
#18882=CARTESIAN_POINT('Ctrl Pts',(-1.86195461813654,1.28333333333333,-1.075));
#18883=CARTESIAN_POINT('Ctrl Pts',(-1.2413030787577,1.34166666666666,-2.15));
#18884=CARTESIAN_POINT('Ctrl Pts',(-1.05319624726672E-15,1.4,-2.15));
#18885=CARTESIAN_POINT('Ctrl Pts',(1.24130307875769,1.45833333333333,-2.15));
#18886=CARTESIAN_POINT('Ctrl Pts',(1.86195461813654,1.51666666666666,-1.075));
#18887=CARTESIAN_POINT('Ctrl Pts',(2.48260615751539,1.575,-1.36814205795513E-15));
#18888=CARTESIAN_POINT('Ctrl Pts',(1.86195461813654,1.63333333333333,1.075));
#18889=CARTESIAN_POINT('Ctrl Pts',(1.2413030787577,1.69166666666666,2.15));
#18890=CARTESIAN_POINT('Ctrl Pts',(1.3164953090834E-15,1.75,2.15));
#18891=CARTESIAN_POINT('Ctrl Pts',(-1.24130307875769,1.80833333333333,2.15));
#18892=CARTESIAN_POINT('Ctrl Pts',(-1.86195461813654,1.86666666666666,1.075));
#18893=CARTESIAN_POINT('Ctrl Pts',(-2.48260615751539,1.925,6.08216805382924E-15));
#18894=CARTESIAN_POINT('Ctrl Pts',(-1.86195461813654,1.98333333333333,-1.075));
#18895=CARTESIAN_POINT('Ctrl Pts',(-1.2413030787577,2.04166666666666,-2.15));
#18896=CARTESIAN_POINT('Ctrl Pts',(-5.39896157561062E-15,2.1,-2.15));
#18897=CARTESIAN_POINT('Ctrl Pts',(1.24130307875769,2.15833333333333,-2.15));
#18898=CARTESIAN_POINT('Ctrl Pts',(1.86195461813654,2.21666666666666,-1.075));
#18899=CARTESIAN_POINT('Ctrl Pts',(2.48260615751539,2.275,-6.38619962226372E-15));
#18900=CARTESIAN_POINT('Ctrl Pts',(1.86195461813655,2.33333333333333,1.07499999999999));
#18901=CARTESIAN_POINT('Ctrl Pts',(1.2413030787577,2.39166666666666,2.15));
#18902=CARTESIAN_POINT('Ctrl Pts',(1.84309343271677E-15,2.45,2.15));
#18903=CARTESIAN_POINT('Ctrl Pts',(-1.24130307875769,2.50833333333333,2.15));
#18904=CARTESIAN_POINT('Ctrl Pts',(-1.86195461813654,2.56666666666666,1.075));
#18905=CARTESIAN_POINT('Ctrl Pts',(-2.48260615751539,2.62499999999999,6.69023119069819E-15));
#18906=CARTESIAN_POINT('Ctrl Pts',(-1.86195461813655,2.68333333333333,-1.07499999999999));
#18907=CARTESIAN_POINT('Ctrl Pts',(-1.2413030787577,2.74166666666666,-2.14999999999999));
#18908=CARTESIAN_POINT('Ctrl Pts',(-2.10639249453345E-15,2.79999999999999,
-2.15));
#18909=CARTESIAN_POINT('Ctrl Pts',(1.24130307875769,2.85833333333333,-2.15));
#18910=CARTESIAN_POINT('Ctrl Pts',(1.86195461813654,2.91666666666666,-1.075));
#18911=CARTESIAN_POINT('Ctrl Pts',(2.48260615751539,2.97499999999999,-6.99426275913266E-15));
#18912=CARTESIAN_POINT('Ctrl Pts',(1.86195461813655,3.03333333333333,1.07499999999999));
#18913=CARTESIAN_POINT('Ctrl Pts',(1.2413030787577,3.09166666666666,2.14999999999999));
#18914=CARTESIAN_POINT('Ctrl Pts',(2.36969155635013E-15,3.14999999999999,
2.15));
#18915=CARTESIAN_POINT('Ctrl Pts',(-1.24130307875769,3.20833333333333,2.15));
#18916=CARTESIAN_POINT('Ctrl Pts',(-1.86195461813654,3.26666666666666,1.075));
#18917=CARTESIAN_POINT('Ctrl Pts',(-2.48260615751539,3.32499999999999,7.29829432756713E-15));
#18918=CARTESIAN_POINT('Ctrl Pts',(-1.86195461813655,3.38333333333333,-1.07499999999999));
#18919=CARTESIAN_POINT('Ctrl Pts',(-1.2413030787577,3.44166666666666,-2.14999999999999));
#18920=CARTESIAN_POINT('Ctrl Pts',(-1.02713250275879E-14,3.49999999999999,
-2.15));
#18921=CARTESIAN_POINT('Ctrl Pts',(1.24130307875769,3.55833333333333,-2.15));
#18922=CARTESIAN_POINT('Ctrl Pts',(1.86195461813654,3.61666666666666,-1.075));
#18923=CARTESIAN_POINT('Ctrl Pts',(2.48260615751539,3.67499999999999,-7.60232589600161E-15));
#18924=CARTESIAN_POINT('Ctrl Pts',(1.86195461813655,3.73333333333333,1.07499999999999));
#18925=CARTESIAN_POINT('Ctrl Pts',(1.2413030787577,3.79166666666666,2.14999999999999));
#18926=CARTESIAN_POINT('Ctrl Pts',(1.05346240894046E-14,3.84999999999999,
2.15));
#18927=CARTESIAN_POINT('Origin',(-1.80160437084306E-13,4.2,2.15));
#18928=CARTESIAN_POINT('Ctrl Pts',(0.,4.28626379701574E-17,2.5));
#18929=CARTESIAN_POINT('Ctrl Pts',(-1.44337567297406,0.0583333333333333,
2.5));
#18930=CARTESIAN_POINT('Ctrl Pts',(-2.1650635094611,0.116666666666666,1.25));
#18931=CARTESIAN_POINT('Ctrl Pts',(-2.88675134594813,0.175,1.76762539787484E-16));
#18932=CARTESIAN_POINT('Ctrl Pts',(-2.1650635094611,0.233333333333333,-1.25));
#18933=CARTESIAN_POINT('Ctrl Pts',(-1.44337567297407,0.291666666666666,
-2.5));
#18934=CARTESIAN_POINT('Ctrl Pts',(-3.06161699786838E-16,0.349999999999999,
-2.5));
#18935=CARTESIAN_POINT('Ctrl Pts',(1.44337567297406,0.408333333333333,-2.5));
#18936=CARTESIAN_POINT('Ctrl Pts',(2.1650635094611,0.466666666666666,-1.25));
#18937=CARTESIAN_POINT('Ctrl Pts',(2.88675134594813,0.524999999999999,-5.30287619362453E-16));
#18938=CARTESIAN_POINT('Ctrl Pts',(2.1650635094611,0.583333333333332,1.25));
#18939=CARTESIAN_POINT('Ctrl Pts',(1.44337567297407,0.641666666666665,2.5));
#18940=CARTESIAN_POINT('Ctrl Pts',(0.,0.699999999999999,2.5));
#18941=CARTESIAN_POINT('Ctrl Pts',(-1.44337567297406,0.758333333333332,
2.5));
#18942=CARTESIAN_POINT('Ctrl Pts',(-2.1650635094611,0.816666666666665,1.25));
#18943=CARTESIAN_POINT('Ctrl Pts',(-2.88675134594813,0.874999999999998,
1.76762539787484E-16));
#18944=CARTESIAN_POINT('Ctrl Pts',(-2.1650635094611,0.933333333333332,-1.25));
#18945=CARTESIAN_POINT('Ctrl Pts',(-1.44337567297407,0.991666666666665,
-2.5));
#18946=CARTESIAN_POINT('Ctrl Pts',(-3.06161699786838E-16,1.05,-2.5));
#18947=CARTESIAN_POINT('Ctrl Pts',(1.44337567297406,1.10833333333333,-2.5));
#18948=CARTESIAN_POINT('Ctrl Pts',(2.1650635094611,1.16666666666666,-1.25));
#18949=CARTESIAN_POINT('Ctrl Pts',(2.88675134594813,1.225,-5.30287619362453E-16));
#18950=CARTESIAN_POINT('Ctrl Pts',(2.1650635094611,1.28333333333333,1.25));
#18951=CARTESIAN_POINT('Ctrl Pts',(1.44337567297407,1.34166666666666,2.5));
#18952=CARTESIAN_POINT('Ctrl Pts',(0.,1.4,2.5));
#18953=CARTESIAN_POINT('Ctrl Pts',(-1.44337567297406,1.45833333333333,2.5));
#18954=CARTESIAN_POINT('Ctrl Pts',(-2.1650635094611,1.51666666666666,1.25));
#18955=CARTESIAN_POINT('Ctrl Pts',(-2.88675134594813,1.575,1.76762539787484E-16));
#18956=CARTESIAN_POINT('Ctrl Pts',(-2.1650635094611,1.63333333333333,-1.25));
#18957=CARTESIAN_POINT('Ctrl Pts',(-1.44337567297407,1.69166666666666,-2.5));
#18958=CARTESIAN_POINT('Ctrl Pts',(-3.06161699786838E-16,1.75,-2.5));
#18959=CARTESIAN_POINT('Ctrl Pts',(1.44337567297406,1.80833333333333,-2.5));
#18960=CARTESIAN_POINT('Ctrl Pts',(2.1650635094611,1.86666666666666,-1.25));
#18961=CARTESIAN_POINT('Ctrl Pts',(2.88675134594813,1.925,-5.30287619362453E-16));
#18962=CARTESIAN_POINT('Ctrl Pts',(2.1650635094611,1.98333333333333,1.25));
#18963=CARTESIAN_POINT('Ctrl Pts',(1.44337567297407,2.04166666666666,2.5));
#18964=CARTESIAN_POINT('Ctrl Pts',(0.,2.1,2.5));
#18965=CARTESIAN_POINT('Ctrl Pts',(-1.44337567297406,2.15833333333333,2.5));
#18966=CARTESIAN_POINT('Ctrl Pts',(-2.1650635094611,2.21666666666666,1.25));
#18967=CARTESIAN_POINT('Ctrl Pts',(-2.88675134594813,2.275,1.76762539787484E-16));
#18968=CARTESIAN_POINT('Ctrl Pts',(-2.1650635094611,2.33333333333333,-1.25));
#18969=CARTESIAN_POINT('Ctrl Pts',(-1.44337567297407,2.39166666666666,-2.5));
#18970=CARTESIAN_POINT('Ctrl Pts',(-3.06161699786838E-16,2.45,-2.5));
#18971=CARTESIAN_POINT('Ctrl Pts',(1.44337567297406,2.50833333333333,-2.5));
#18972=CARTESIAN_POINT('Ctrl Pts',(2.1650635094611,2.56666666666666,-1.25));
#18973=CARTESIAN_POINT('Ctrl Pts',(2.88675134594813,2.62499999999999,-5.30287619362453E-16));
#18974=CARTESIAN_POINT('Ctrl Pts',(2.1650635094611,2.68333333333333,1.25));
#18975=CARTESIAN_POINT('Ctrl Pts',(1.44337567297407,2.74166666666666,2.5));
#18976=CARTESIAN_POINT('Ctrl Pts',(0.,2.79999999999999,2.5));
#18977=CARTESIAN_POINT('Ctrl Pts',(-1.44337567297406,2.85833333333333,2.5));
#18978=CARTESIAN_POINT('Ctrl Pts',(-2.1650635094611,2.91666666666666,1.25));
#18979=CARTESIAN_POINT('Ctrl Pts',(-2.88675134594813,2.97499999999999,1.76762539787484E-16));
#18980=CARTESIAN_POINT('Ctrl Pts',(-2.1650635094611,3.03333333333333,-1.25));
#18981=CARTESIAN_POINT('Ctrl Pts',(-1.44337567297407,3.09166666666666,-2.5));
#18982=CARTESIAN_POINT('Ctrl Pts',(-3.06161699786838E-16,3.14999999999999,
-2.5));
#18983=CARTESIAN_POINT('Ctrl Pts',(1.44337567297406,3.20833333333333,-2.5));
#18984=CARTESIAN_POINT('Ctrl Pts',(2.1650635094611,3.26666666666666,-1.25));
#18985=CARTESIAN_POINT('Ctrl Pts',(2.88675134594813,3.32499999999999,-5.30287619362453E-16));
#18986=CARTESIAN_POINT('Ctrl Pts',(2.1650635094611,3.38333333333333,1.25));
#18987=CARTESIAN_POINT('Ctrl Pts',(1.44337567297407,3.44166666666666,2.5));
#18988=CARTESIAN_POINT('Ctrl Pts',(0.,3.49999999999999,2.5));
#18989=CARTESIAN_POINT('Ctrl Pts',(-1.44337567297406,3.55833333333333,2.5));
#18990=CARTESIAN_POINT('Ctrl Pts',(-2.1650635094611,3.61666666666666,1.25));
#18991=CARTESIAN_POINT('Ctrl Pts',(-2.88675134594813,3.67499999999999,1.76762539787484E-16));
#18992=CARTESIAN_POINT('Ctrl Pts',(-2.1650635094611,3.73333333333333,-1.25));
#18993=CARTESIAN_POINT('Ctrl Pts',(-1.44337567297407,3.79166666666666,-2.5));
#18994=CARTESIAN_POINT('Ctrl Pts',(-3.06161699786838E-16,3.84999999999999,
-2.5));
#18995=CARTESIAN_POINT('Ctrl Pts',(1.44337567297406,3.90833333333333,-2.5));
#18996=CARTESIAN_POINT('Ctrl Pts',(2.1650635094611,3.96666666666666,-1.25));
#18997=CARTESIAN_POINT('Ctrl Pts',(2.88675134594813,4.02499999999999,-5.30287619362453E-16));
#18998=CARTESIAN_POINT('Ctrl Pts',(2.1650635094611,4.08333333333333,1.25));
#18999=CARTESIAN_POINT('Ctrl Pts',(1.44337567297407,4.14166666666666,2.5));
#19000=CARTESIAN_POINT('Ctrl Pts',(0.,4.19999999999999,2.5));
#19001=CARTESIAN_POINT('Ctrl Pts',(0.,-0.205025253169417,2.5));
#19002=CARTESIAN_POINT('Ctrl Pts',(-1.44337567297406,-0.146691919836083,
2.5));
#19003=CARTESIAN_POINT('Ctrl Pts',(-2.1650635094611,-0.0883585865027503,
1.25));
#19004=CARTESIAN_POINT('Ctrl Pts',(-2.88675134594813,-0.0300252531694171,
1.76762539787484E-16));
#19005=CARTESIAN_POINT('Ctrl Pts',(-2.1650635094611,0.0283080801639162,
-1.25));
#19006=CARTESIAN_POINT('Ctrl Pts',(-1.44337567297407,0.0866414134972494,
-2.5));
#19007=CARTESIAN_POINT('Ctrl Pts',(-3.06161699786838E-16,0.144974746830583,
-2.5));
#19008=CARTESIAN_POINT('Ctrl Pts',(1.44337567297406,0.203308080163916,-2.5));
#19009=CARTESIAN_POINT('Ctrl Pts',(2.1650635094611,0.261641413497249,-1.25));
#19010=CARTESIAN_POINT('Ctrl Pts',(2.88675134594813,0.319974746830582,-5.30287619362453E-16));
#19011=CARTESIAN_POINT('Ctrl Pts',(2.1650635094611,0.378308080163915,1.25));
#19012=CARTESIAN_POINT('Ctrl Pts',(1.44337567297407,0.436641413497249,2.5));
#19013=CARTESIAN_POINT('Ctrl Pts',(0.,0.494974746830582,2.5));
#19014=CARTESIAN_POINT('Ctrl Pts',(-1.44337567297406,0.553308080163915,
2.5));
#19015=CARTESIAN_POINT('Ctrl Pts',(-2.1650635094611,0.611641413497248,1.25));
#19016=CARTESIAN_POINT('Ctrl Pts',(-2.88675134594813,0.669974746830582,
1.76762539787484E-16));
#19017=CARTESIAN_POINT('Ctrl Pts',(-2.1650635094611,0.728308080163915,-1.25));
#19018=CARTESIAN_POINT('Ctrl Pts',(-1.44337567297407,0.786641413497248,
-2.5));
#19019=CARTESIAN_POINT('Ctrl Pts',(-3.06161699786838E-16,0.844974746830581,
-2.5));
#19020=CARTESIAN_POINT('Ctrl Pts',(1.44337567297406,0.903308080163914,-2.5));
#19021=CARTESIAN_POINT('Ctrl Pts',(2.1650635094611,0.961641413497248,-1.25));
#19022=CARTESIAN_POINT('Ctrl Pts',(2.88675134594813,1.01997474683058,-5.30287619362453E-16));
#19023=CARTESIAN_POINT('Ctrl Pts',(2.1650635094611,1.07830808016391,1.25));
#19024=CARTESIAN_POINT('Ctrl Pts',(1.44337567297407,1.13664141349725,2.5));
#19025=CARTESIAN_POINT('Ctrl Pts',(0.,1.19497474683058,2.5));
#19026=CARTESIAN_POINT('Ctrl Pts',(-1.44337567297406,1.25330808016391,2.5));
#19027=CARTESIAN_POINT('Ctrl Pts',(-2.1650635094611,1.31164141349725,1.25));
#19028=CARTESIAN_POINT('Ctrl Pts',(-2.88675134594813,1.36997474683058,1.76762539787484E-16));
#19029=CARTESIAN_POINT('Ctrl Pts',(-2.1650635094611,1.42830808016391,-1.25));
#19030=CARTESIAN_POINT('Ctrl Pts',(-1.44337567297407,1.48664141349725,-2.5));
#19031=CARTESIAN_POINT('Ctrl Pts',(-3.06161699786838E-16,1.54497474683058,
-2.5));
#19032=CARTESIAN_POINT('Ctrl Pts',(1.44337567297406,1.60330808016391,-2.5));
#19033=CARTESIAN_POINT('Ctrl Pts',(2.1650635094611,1.66164141349725,-1.25));
#19034=CARTESIAN_POINT('Ctrl Pts',(2.88675134594813,1.71997474683058,-5.30287619362453E-16));
#19035=CARTESIAN_POINT('Ctrl Pts',(2.1650635094611,1.77830808016391,1.25));
#19036=CARTESIAN_POINT('Ctrl Pts',(1.44337567297407,1.83664141349725,2.5));
#19037=CARTESIAN_POINT('Ctrl Pts',(0.,1.89497474683058,2.5));
#19038=CARTESIAN_POINT('Ctrl Pts',(-1.44337567297406,1.95330808016391,2.5));
#19039=CARTESIAN_POINT('Ctrl Pts',(-2.1650635094611,2.01164141349725,1.25));
#19040=CARTESIAN_POINT('Ctrl Pts',(-2.88675134594813,2.06997474683058,1.76762539787484E-16));
#19041=CARTESIAN_POINT('Ctrl Pts',(-2.1650635094611,2.12830808016391,-1.25));
#19042=CARTESIAN_POINT('Ctrl Pts',(-1.44337567297407,2.18664141349725,-2.5));
#19043=CARTESIAN_POINT('Ctrl Pts',(-3.06161699786838E-16,2.24497474683058,
-2.5));
#19044=CARTESIAN_POINT('Ctrl Pts',(1.44337567297406,2.30330808016391,-2.5));
#19045=CARTESIAN_POINT('Ctrl Pts',(2.1650635094611,2.36164141349724,-1.25));
#19046=CARTESIAN_POINT('Ctrl Pts',(2.88675134594813,2.41997474683058,-5.30287619362453E-16));
#19047=CARTESIAN_POINT('Ctrl Pts',(2.1650635094611,2.47830808016391,1.25));
#19048=CARTESIAN_POINT('Ctrl Pts',(1.44337567297407,2.53664141349724,2.5));
#19049=CARTESIAN_POINT('Ctrl Pts',(0.,2.59497474683058,2.5));
#19050=CARTESIAN_POINT('Ctrl Pts',(-1.44337567297406,2.65330808016391,2.5));
#19051=CARTESIAN_POINT('Ctrl Pts',(-2.1650635094611,2.71164141349724,1.25));
#19052=CARTESIAN_POINT('Ctrl Pts',(-2.88675134594813,2.76997474683058,1.76762539787484E-16));
#19053=CARTESIAN_POINT('Ctrl Pts',(-2.1650635094611,2.82830808016391,-1.25));
#19054=CARTESIAN_POINT('Ctrl Pts',(-1.44337567297407,2.88664141349724,-2.5));
#19055=CARTESIAN_POINT('Ctrl Pts',(-3.06161699786838E-16,2.94497474683058,
-2.5));
#19056=CARTESIAN_POINT('Ctrl Pts',(1.44337567297406,3.00330808016391,-2.5));
#19057=CARTESIAN_POINT('Ctrl Pts',(2.1650635094611,3.06164141349724,-1.25));
#19058=CARTESIAN_POINT('Ctrl Pts',(2.88675134594813,3.11997474683058,-5.30287619362453E-16));
#19059=CARTESIAN_POINT('Ctrl Pts',(2.1650635094611,3.17830808016391,1.25));
#19060=CARTESIAN_POINT('Ctrl Pts',(1.44337567297407,3.23664141349724,2.5));
#19061=CARTESIAN_POINT('Ctrl Pts',(0.,3.29497474683058,2.5));
#19062=CARTESIAN_POINT('Ctrl Pts',(-1.44337567297406,3.35330808016391,2.5));
#19063=CARTESIAN_POINT('Ctrl Pts',(-2.1650635094611,3.41164141349724,1.25));
#19064=CARTESIAN_POINT('Ctrl Pts',(-2.88675134594813,3.46997474683058,1.76762539787484E-16));
#19065=CARTESIAN_POINT('Ctrl Pts',(-2.1650635094611,3.52830808016391,-1.25));
#19066=CARTESIAN_POINT('Ctrl Pts',(-1.44337567297407,3.58664141349724,-2.5));
#19067=CARTESIAN_POINT('Ctrl Pts',(-3.06161699786838E-16,3.64497474683058,
-2.5));
#19068=CARTESIAN_POINT('Ctrl Pts',(1.44337567297406,3.70330808016391,-2.5));
#19069=CARTESIAN_POINT('Ctrl Pts',(2.1650635094611,3.76164141349724,-1.25));
#19070=CARTESIAN_POINT('Ctrl Pts',(2.88675134594813,3.81997474683058,-5.30287619362453E-16));
#19071=CARTESIAN_POINT('Ctrl Pts',(2.1650635094611,3.87830808016391,1.25));
#19072=CARTESIAN_POINT('Ctrl Pts',(1.44337567297407,3.93664141349724,2.5));
#19073=CARTESIAN_POINT('Ctrl Pts',(0.,3.99497474683058,2.5));
#19074=CARTESIAN_POINT('Ctrl Pts',(0.,-0.35,2.35502525316942));
#19075=CARTESIAN_POINT('Ctrl Pts',(-1.35967446386573,-0.291666666666667,
2.35502525316942));
#19076=CARTESIAN_POINT('Ctrl Pts',(-2.03951169579859,-0.233333333333334,
1.17751262658471));
#19077=CARTESIAN_POINT('Ctrl Pts',(-2.71934892773146,-0.175,1.66512098005556E-16));
#19078=CARTESIAN_POINT('Ctrl Pts',(-2.03951169579859,-0.116666666666667,
-1.17751262658471));
#19079=CARTESIAN_POINT('Ctrl Pts',(-1.35967446386573,-0.0583333333333339,
-2.35502525316942));
#19080=CARTESIAN_POINT('Ctrl Pts',(-2.88407413820511E-16,-7.04731412115578E-16,
-2.35502525316942));
#19081=CARTESIAN_POINT('Ctrl Pts',(1.35967446386573,0.0583333333333326,
-2.35502525316942));
#19082=CARTESIAN_POINT('Ctrl Pts',(2.03951169579859,0.116666666666666,-1.17751262658471));
#19083=CARTESIAN_POINT('Ctrl Pts',(2.71934892773146,0.174999999999999,-4.99536294016668E-16));
#19084=CARTESIAN_POINT('Ctrl Pts',(2.03951169579859,0.233333333333332,1.17751262658471));
#19085=CARTESIAN_POINT('Ctrl Pts',(1.35967446386573,0.291666666666665,2.35502525316942));
#19086=CARTESIAN_POINT('Ctrl Pts',(0.,0.349999999999999,2.35502525316942));
#19087=CARTESIAN_POINT('Ctrl Pts',(-1.35967446386573,0.408333333333332,
2.35502525316942));
#19088=CARTESIAN_POINT('Ctrl Pts',(-2.03951169579859,0.466666666666665,
1.17751262658471));
#19089=CARTESIAN_POINT('Ctrl Pts',(-2.71934892773146,0.524999999999998,
1.66512098005556E-16));
#19090=CARTESIAN_POINT('Ctrl Pts',(-2.03951169579859,0.583333333333332,
-1.17751262658471));
#19091=CARTESIAN_POINT('Ctrl Pts',(-1.35967446386573,0.641666666666665,
-2.35502525316942));
#19092=CARTESIAN_POINT('Ctrl Pts',(-2.88407413820511E-16,0.699999999999998,
-2.35502525316942));
#19093=CARTESIAN_POINT('Ctrl Pts',(1.35967446386573,0.758333333333331,-2.35502525316942));
#19094=CARTESIAN_POINT('Ctrl Pts',(2.03951169579859,0.816666666666664,-1.17751262658471));
#19095=CARTESIAN_POINT('Ctrl Pts',(2.71934892773146,0.874999999999998,-4.99536294016668E-16));
#19096=CARTESIAN_POINT('Ctrl Pts',(2.03951169579859,0.933333333333331,1.17751262658471));
#19097=CARTESIAN_POINT('Ctrl Pts',(1.35967446386573,0.991666666666664,2.35502525316942));
#19098=CARTESIAN_POINT('Ctrl Pts',(0.,1.05,2.35502525316942));
#19099=CARTESIAN_POINT('Ctrl Pts',(-1.35967446386573,1.10833333333333,2.35502525316942));
#19100=CARTESIAN_POINT('Ctrl Pts',(-2.03951169579859,1.16666666666666,1.17751262658471));
#19101=CARTESIAN_POINT('Ctrl Pts',(-2.71934892773146,1.225,1.66512098005556E-16));
#19102=CARTESIAN_POINT('Ctrl Pts',(-2.03951169579859,1.28333333333333,-1.17751262658471));
#19103=CARTESIAN_POINT('Ctrl Pts',(-1.35967446386573,1.34166666666666,-2.35502525316942));
#19104=CARTESIAN_POINT('Ctrl Pts',(-2.88407413820511E-16,1.4,-2.35502525316942));
#19105=CARTESIAN_POINT('Ctrl Pts',(1.35967446386573,1.45833333333333,-2.35502525316942));
#19106=CARTESIAN_POINT('Ctrl Pts',(2.03951169579859,1.51666666666666,-1.17751262658471));
#19107=CARTESIAN_POINT('Ctrl Pts',(2.71934892773146,1.575,-4.99536294016668E-16));
#19108=CARTESIAN_POINT('Ctrl Pts',(2.03951169579859,1.63333333333333,1.17751262658471));
#19109=CARTESIAN_POINT('Ctrl Pts',(1.35967446386573,1.69166666666666,2.35502525316942));
#19110=CARTESIAN_POINT('Ctrl Pts',(0.,1.75,2.35502525316942));
#19111=CARTESIAN_POINT('Ctrl Pts',(-1.35967446386573,1.80833333333333,2.35502525316942));
#19112=CARTESIAN_POINT('Ctrl Pts',(-2.03951169579859,1.86666666666666,1.17751262658471));
#19113=CARTESIAN_POINT('Ctrl Pts',(-2.71934892773146,1.925,1.66512098005556E-16));
#19114=CARTESIAN_POINT('Ctrl Pts',(-2.03951169579859,1.98333333333333,-1.17751262658471));
#19115=CARTESIAN_POINT('Ctrl Pts',(-1.35967446386573,2.04166666666666,-2.35502525316942));
#19116=CARTESIAN_POINT('Ctrl Pts',(-2.88407413820511E-16,2.09999999999999,
-2.35502525316942));
#19117=CARTESIAN_POINT('Ctrl Pts',(1.35967446386573,2.15833333333333,-2.35502525316942));
#19118=CARTESIAN_POINT('Ctrl Pts',(2.03951169579859,2.21666666666666,-1.17751262658471));
#19119=CARTESIAN_POINT('Ctrl Pts',(2.71934892773146,2.275,-4.99536294016668E-16));
#19120=CARTESIAN_POINT('Ctrl Pts',(2.03951169579859,2.33333333333333,1.17751262658471));
#19121=CARTESIAN_POINT('Ctrl Pts',(1.35967446386573,2.39166666666666,2.35502525316942));
#19122=CARTESIAN_POINT('Ctrl Pts',(0.,2.44999999999999,2.35502525316942));
#19123=CARTESIAN_POINT('Ctrl Pts',(-1.35967446386573,2.50833333333333,2.35502525316942));
#19124=CARTESIAN_POINT('Ctrl Pts',(-2.03951169579859,2.56666666666666,1.17751262658471));
#19125=CARTESIAN_POINT('Ctrl Pts',(-2.71934892773146,2.62499999999999,1.66512098005556E-16));
#19126=CARTESIAN_POINT('Ctrl Pts',(-2.03951169579859,2.68333333333333,-1.17751262658471));
#19127=CARTESIAN_POINT('Ctrl Pts',(-1.35967446386573,2.74166666666666,-2.35502525316942));
#19128=CARTESIAN_POINT('Ctrl Pts',(-2.88407413820511E-16,2.79999999999999,
-2.35502525316942));
#19129=CARTESIAN_POINT('Ctrl Pts',(1.35967446386573,2.85833333333333,-2.35502525316942));
#19130=CARTESIAN_POINT('Ctrl Pts',(2.03951169579859,2.91666666666666,-1.17751262658471));
#19131=CARTESIAN_POINT('Ctrl Pts',(2.71934892773146,2.97499999999999,-4.99536294016668E-16));
#19132=CARTESIAN_POINT('Ctrl Pts',(2.03951169579859,3.03333333333333,1.17751262658471));
#19133=CARTESIAN_POINT('Ctrl Pts',(1.35967446386573,3.09166666666666,2.35502525316942));
#19134=CARTESIAN_POINT('Ctrl Pts',(0.,3.14999999999999,2.35502525316942));
#19135=CARTESIAN_POINT('Ctrl Pts',(-1.35967446386573,3.20833333333333,2.35502525316942));
#19136=CARTESIAN_POINT('Ctrl Pts',(-2.03951169579859,3.26666666666666,1.17751262658471));
#19137=CARTESIAN_POINT('Ctrl Pts',(-2.71934892773146,3.32499999999999,1.66512098005556E-16));
#19138=CARTESIAN_POINT('Ctrl Pts',(-2.03951169579859,3.38333333333333,-1.17751262658471));
#19139=CARTESIAN_POINT('Ctrl Pts',(-1.35967446386573,3.44166666666666,-2.35502525316942));
#19140=CARTESIAN_POINT('Ctrl Pts',(-2.88407413820511E-16,3.49999999999999,
-2.35502525316942));
#19141=CARTESIAN_POINT('Ctrl Pts',(1.35967446386573,3.55833333333333,-2.35502525316942));
#19142=CARTESIAN_POINT('Ctrl Pts',(2.03951169579859,3.61666666666666,-1.17751262658471));
#19143=CARTESIAN_POINT('Ctrl Pts',(2.71934892773146,3.67499999999999,-4.99536294016668E-16));
#19144=CARTESIAN_POINT('Ctrl Pts',(2.03951169579859,3.73333333333332,1.17751262658471));
#19145=CARTESIAN_POINT('Ctrl Pts',(1.35967446386573,3.79166666666666,2.35502525316942));
#19146=CARTESIAN_POINT('Ctrl Pts',(0.,3.84999999999999,2.35502525316942));
#19147=CARTESIAN_POINT('Ctrl Pts',(0.,-0.35,2.15));
#19148=CARTESIAN_POINT('Ctrl Pts',(-1.2413030787577,-0.291666666666667,
2.15));
#19149=CARTESIAN_POINT('Ctrl Pts',(-1.86195461813654,-0.233333333333334,
1.075));
#19150=CARTESIAN_POINT('Ctrl Pts',(-2.48260615751539,-0.175,1.52015784217237E-16));
#19151=CARTESIAN_POINT('Ctrl Pts',(-1.86195461813654,-0.116666666666667,
-1.075));
#19152=CARTESIAN_POINT('Ctrl Pts',(-1.2413030787577,-0.058333333333334,
-2.15));
#19153=CARTESIAN_POINT('Ctrl Pts',(-2.63299061816681E-16,-7.58941520739853E-16,
-2.15));
#19154=CARTESIAN_POINT('Ctrl Pts',(1.24130307875769,0.0583333333333325,
-2.15));
#19155=CARTESIAN_POINT('Ctrl Pts',(1.86195461813654,0.116666666666666,-1.075));
#19156=CARTESIAN_POINT('Ctrl Pts',(2.48260615751539,0.174999999999999,-4.5604735265171E-16));
#19157=CARTESIAN_POINT('Ctrl Pts',(1.86195461813654,0.233333333333332,1.075));
#19158=CARTESIAN_POINT('Ctrl Pts',(1.2413030787577,0.291666666666665,2.15));
#19159=CARTESIAN_POINT('Ctrl Pts',(0.,0.349999999999999,2.15));
#19160=CARTESIAN_POINT('Ctrl Pts',(-1.2413030787577,0.408333333333332,2.15));
#19161=CARTESIAN_POINT('Ctrl Pts',(-1.86195461813654,0.466666666666665,
1.075));
#19162=CARTESIAN_POINT('Ctrl Pts',(-2.48260615751539,0.524999999999998,
1.52015784217237E-16));
#19163=CARTESIAN_POINT('Ctrl Pts',(-1.86195461813654,0.583333333333331,
-1.075));
#19164=CARTESIAN_POINT('Ctrl Pts',(-1.2413030787577,0.641666666666665,-2.15));
#19165=CARTESIAN_POINT('Ctrl Pts',(-2.63299061816681E-16,0.699999999999998,
-2.15));
#19166=CARTESIAN_POINT('Ctrl Pts',(1.24130307875769,0.758333333333331,-2.15));
#19167=CARTESIAN_POINT('Ctrl Pts',(1.86195461813654,0.816666666666664,-1.075));
#19168=CARTESIAN_POINT('Ctrl Pts',(2.48260615751539,0.874999999999997,-4.5604735265171E-16));
#19169=CARTESIAN_POINT('Ctrl Pts',(1.86195461813654,0.933333333333331,1.075));
#19170=CARTESIAN_POINT('Ctrl Pts',(1.2413030787577,0.991666666666664,2.15));
#19171=CARTESIAN_POINT('Ctrl Pts',(0.,1.05,2.15));
#19172=CARTESIAN_POINT('Ctrl Pts',(-1.2413030787577,1.10833333333333,2.15));
#19173=CARTESIAN_POINT('Ctrl Pts',(-1.86195461813654,1.16666666666666,1.075));
#19174=CARTESIAN_POINT('Ctrl Pts',(-2.48260615751539,1.225,1.52015784217237E-16));
#19175=CARTESIAN_POINT('Ctrl Pts',(-1.86195461813654,1.28333333333333,-1.075));
#19176=CARTESIAN_POINT('Ctrl Pts',(-1.2413030787577,1.34166666666666,-2.15));
#19177=CARTESIAN_POINT('Ctrl Pts',(-2.63299061816681E-16,1.4,-2.15));
#19178=CARTESIAN_POINT('Ctrl Pts',(1.24130307875769,1.45833333333333,-2.15));
#19179=CARTESIAN_POINT('Ctrl Pts',(1.86195461813654,1.51666666666666,-1.075));
#19180=CARTESIAN_POINT('Ctrl Pts',(2.48260615751539,1.575,-4.5604735265171E-16));
#19181=CARTESIAN_POINT('Ctrl Pts',(1.86195461813654,1.63333333333333,1.075));
#19182=CARTESIAN_POINT('Ctrl Pts',(1.2413030787577,1.69166666666666,2.15));
#19183=CARTESIAN_POINT('Ctrl Pts',(0.,1.75,2.15));
#19184=CARTESIAN_POINT('Ctrl Pts',(-1.2413030787577,1.80833333333333,2.15));
#19185=CARTESIAN_POINT('Ctrl Pts',(-1.86195461813654,1.86666666666666,1.075));
#19186=CARTESIAN_POINT('Ctrl Pts',(-2.48260615751539,1.925,1.52015784217237E-16));
#19187=CARTESIAN_POINT('Ctrl Pts',(-1.86195461813654,1.98333333333333,-1.075));
#19188=CARTESIAN_POINT('Ctrl Pts',(-1.2413030787577,2.04166666666666,-2.15));
#19189=CARTESIAN_POINT('Ctrl Pts',(-2.63299061816681E-16,2.1,-2.15));
#19190=CARTESIAN_POINT('Ctrl Pts',(1.24130307875769,2.15833333333333,-2.15));
#19191=CARTESIAN_POINT('Ctrl Pts',(1.86195461813654,2.21666666666666,-1.075));
#19192=CARTESIAN_POINT('Ctrl Pts',(2.48260615751539,2.275,-4.5604735265171E-16));
#19193=CARTESIAN_POINT('Ctrl Pts',(1.86195461813654,2.33333333333333,1.075));
#19194=CARTESIAN_POINT('Ctrl Pts',(1.2413030787577,2.39166666666666,2.15));
#19195=CARTESIAN_POINT('Ctrl Pts',(0.,2.44999999999999,2.15));
#19196=CARTESIAN_POINT('Ctrl Pts',(-1.2413030787577,2.50833333333333,2.15));
#19197=CARTESIAN_POINT('Ctrl Pts',(-1.86195461813654,2.56666666666666,1.075));
#19198=CARTESIAN_POINT('Ctrl Pts',(-2.48260615751539,2.62499999999999,1.52015784217237E-16));
#19199=CARTESIAN_POINT('Ctrl Pts',(-1.86195461813654,2.68333333333333,-1.075));
#19200=CARTESIAN_POINT('Ctrl Pts',(-1.2413030787577,2.74166666666666,-2.15));
#19201=CARTESIAN_POINT('Ctrl Pts',(-2.63299061816681E-16,2.79999999999999,
-2.15));
#19202=CARTESIAN_POINT('Ctrl Pts',(1.24130307875769,2.85833333333333,-2.15));
#19203=CARTESIAN_POINT('Ctrl Pts',(1.86195461813654,2.91666666666666,-1.075));
#19204=CARTESIAN_POINT('Ctrl Pts',(2.48260615751539,2.97499999999999,-4.5604735265171E-16));
#19205=CARTESIAN_POINT('Ctrl Pts',(1.86195461813654,3.03333333333333,1.075));
#19206=CARTESIAN_POINT('Ctrl Pts',(1.2413030787577,3.09166666666666,2.15));
#19207=CARTESIAN_POINT('Ctrl Pts',(0.,3.14999999999999,2.15));
#19208=CARTESIAN_POINT('Ctrl Pts',(-1.2413030787577,3.20833333333333,2.15));
#19209=CARTESIAN_POINT('Ctrl Pts',(-1.86195461813654,3.26666666666666,1.075));
#19210=CARTESIAN_POINT('Ctrl Pts',(-2.48260615751539,3.32499999999999,1.52015784217237E-16));
#19211=CARTESIAN_POINT('Ctrl Pts',(-1.86195461813654,3.38333333333333,-1.075));
#19212=CARTESIAN_POINT('Ctrl Pts',(-1.2413030787577,3.44166666666666,-2.15));
#19213=CARTESIAN_POINT('Ctrl Pts',(-2.63299061816681E-16,3.49999999999999,
-2.15));
#19214=CARTESIAN_POINT('Ctrl Pts',(1.24130307875769,3.55833333333333,-2.15));
#19215=CARTESIAN_POINT('Ctrl Pts',(1.86195461813654,3.61666666666666,-1.075));
#19216=CARTESIAN_POINT('Ctrl Pts',(2.48260615751539,3.67499999999999,-4.5604735265171E-16));
#19217=CARTESIAN_POINT('Ctrl Pts',(1.86195461813654,3.73333333333333,1.075));
#19218=CARTESIAN_POINT('Ctrl Pts',(1.2413030787577,3.79166666666666,2.15));
#19219=CARTESIAN_POINT('Ctrl Pts',(0.,3.84999999999999,2.15));
#19220=CARTESIAN_POINT('',(0.,4.28626379701574E-17,2.5));
#19221=CARTESIAN_POINT('Origin',(0.,0.,2.15));
#19222=CARTESIAN_POINT('',(-1.02907469966573E-13,4.2,2.5));
#19223=CARTESIAN_POINT('Ctrl Pts',(0.,4.28626379701574E-17,2.5));
#19224=CARTESIAN_POINT('Ctrl Pts',(-1.44337567297406,0.0583333333333333,
2.5));
#19225=CARTESIAN_POINT('Ctrl Pts',(-2.1650635094611,0.116666666666666,1.25));
#19226=CARTESIAN_POINT('Ctrl Pts',(-2.88675134594813,0.175,1.76762539787484E-16));
#19227=CARTESIAN_POINT('Ctrl Pts',(-2.1650635094611,0.233333333333333,-1.25));
#19228=CARTESIAN_POINT('Ctrl Pts',(-1.44337567297407,0.291666666666666,
-2.5));
#19229=CARTESIAN_POINT('Ctrl Pts',(-3.06161699786838E-16,0.349999999999999,
-2.5));
#19230=CARTESIAN_POINT('Ctrl Pts',(1.44337567297406,0.408333333333333,-2.5));
#19231=CARTESIAN_POINT('Ctrl Pts',(2.1650635094611,0.466666666666666,-1.25));
#19232=CARTESIAN_POINT('Ctrl Pts',(2.88675134594813,0.524999999999999,-5.30287619362453E-16));
#19233=CARTESIAN_POINT('Ctrl Pts',(2.1650635094611,0.583333333333332,1.25));
#19234=CARTESIAN_POINT('Ctrl Pts',(1.44337567297407,0.641666666666665,2.5));
#19235=CARTESIAN_POINT('Ctrl Pts',(6.12323399573677E-16,0.699999999999999,
2.5));
#19236=CARTESIAN_POINT('Ctrl Pts',(-1.44337567297406,0.758333333333332,
2.5));
#19237=CARTESIAN_POINT('Ctrl Pts',(-2.1650635094611,0.816666666666665,1.25));
#19238=CARTESIAN_POINT('Ctrl Pts',(-2.88675134594813,0.874999999999998,
3.44776294744884E-15));
#19239=CARTESIAN_POINT('Ctrl Pts',(-2.1650635094611,0.933333333333332,-1.25));
#19240=CARTESIAN_POINT('Ctrl Pts',(-1.44337567297407,0.991666666666665,
-2.5));
#19241=CARTESIAN_POINT('Ctrl Pts',(-9.18485099360515E-16,1.05,-2.5));
#19242=CARTESIAN_POINT('Ctrl Pts',(1.44337567297406,1.10833333333333,-2.5));
#19243=CARTESIAN_POINT('Ctrl Pts',(2.16506350946109,1.16666666666666,-1.25));
#19244=CARTESIAN_POINT('Ctrl Pts',(2.88675134594813,1.225,-1.23733777851239E-15));
#19245=CARTESIAN_POINT('Ctrl Pts',(2.1650635094611,1.28333333333333,1.25));
#19246=CARTESIAN_POINT('Ctrl Pts',(1.44337567297407,1.34166666666666,2.5));
#19247=CARTESIAN_POINT('Ctrl Pts',(1.22464679914735E-15,1.4,2.5));
#19248=CARTESIAN_POINT('Ctrl Pts',(-1.44337567297406,1.45833333333333,2.5));
#19249=CARTESIAN_POINT('Ctrl Pts',(-2.16506350946109,1.51666666666666,1.25));
#19250=CARTESIAN_POINT('Ctrl Pts',(-2.88675134594813,1.575,6.7187633551102E-15));
#19251=CARTESIAN_POINT('Ctrl Pts',(-2.1650635094611,1.63333333333333,-1.25));
#19252=CARTESIAN_POINT('Ctrl Pts',(-1.44337567297407,1.69166666666666,-2.5));
#19253=CARTESIAN_POINT('Ctrl Pts',(-5.97170059743482E-15,1.75,-2.5));
#19254=CARTESIAN_POINT('Ctrl Pts',(1.44337567297406,1.80833333333333,-2.5));
#19255=CARTESIAN_POINT('Ctrl Pts',(2.16506350946109,1.86666666666666,-1.25));
#19256=CARTESIAN_POINT('Ctrl Pts',(2.88675134594813,1.925,-7.07228843468517E-15));
#19257=CARTESIAN_POINT('Ctrl Pts',(2.1650635094611,1.98333333333333,1.24999999999999));
#19258=CARTESIAN_POINT('Ctrl Pts',(1.44337567297407,2.04166666666666,2.49999999999999));
#19259=CARTESIAN_POINT('Ctrl Pts',(1.83697019872103E-15,2.1,2.5));
#19260=CARTESIAN_POINT('Ctrl Pts',(-1.44337567297406,2.15833333333333,2.5));
#19261=CARTESIAN_POINT('Ctrl Pts',(-2.16506350946109,2.21666666666666,1.25));
#19262=CARTESIAN_POINT('Ctrl Pts',(-2.88675134594813,2.275,7.42581351426014E-15));
#19263=CARTESIAN_POINT('Ctrl Pts',(-2.1650635094611,2.33333333333333,-1.24999999999999));
#19264=CARTESIAN_POINT('Ctrl Pts',(-1.44337567297407,2.39166666666666,-2.49999999999999));
#19265=CARTESIAN_POINT('Ctrl Pts',(-2.14313189850787E-15,2.45,-2.5));
#19266=CARTESIAN_POINT('Ctrl Pts',(1.44337567297406,2.50833333333333,-2.5));
#19267=CARTESIAN_POINT('Ctrl Pts',(2.16506350946109,2.56666666666666,-1.25));
#19268=CARTESIAN_POINT('Ctrl Pts',(2.88675134594813,2.625,-7.7793385938351E-15));
#19269=CARTESIAN_POINT('Ctrl Pts',(2.1650635094611,2.68333333333333,1.24999999999999));
#19270=CARTESIAN_POINT('Ctrl Pts',(1.44337567297407,2.74166666666666,2.49999999999999));
#19271=CARTESIAN_POINT('Ctrl Pts',(2.44929359829471E-15,2.79999999999999,
2.5));
#19272=CARTESIAN_POINT('Ctrl Pts',(-1.44337567297406,2.85833333333333,2.5));
#19273=CARTESIAN_POINT('Ctrl Pts',(-2.16506350946109,2.91666666666666,1.25));
#19274=CARTESIAN_POINT('Ctrl Pts',(-2.88675134594813,2.97499999999999,8.13286367341007E-15));
#19275=CARTESIAN_POINT('Ctrl Pts',(-2.1650635094611,3.03333333333333,-1.24999999999999));
#19276=CARTESIAN_POINT('Ctrl Pts',(-1.44337567297407,3.09166666666666,-2.49999999999999));
#19277=CARTESIAN_POINT('Ctrl Pts',(-1.16372394950828E-14,3.14999999999999,
-2.5));
#19278=CARTESIAN_POINT('Ctrl Pts',(1.44337567297406,3.20833333333333,-2.5));
#19279=CARTESIAN_POINT('Ctrl Pts',(2.16506350946109,3.26666666666666,-1.25000000000001));
#19280=CARTESIAN_POINT('Ctrl Pts',(2.88675134594813,3.32499999999999,-8.48638875298504E-15));
#19281=CARTESIAN_POINT('Ctrl Pts',(2.1650635094611,3.38333333333333,1.24999999999999));
#19282=CARTESIAN_POINT('Ctrl Pts',(1.44337567297407,3.44166666666666,2.49999999999999));
#19283=CARTESIAN_POINT('Ctrl Pts',(1.19434011948696E-14,3.49999999999999,
2.5));
#19284=CARTESIAN_POINT('Ctrl Pts',(-1.44337567297406,3.55833333333333,2.5));
#19285=CARTESIAN_POINT('Ctrl Pts',(-2.16506350946109,3.61666666666666,1.25000000000001));
#19286=CARTESIAN_POINT('Ctrl Pts',(-2.88675134594813,3.67499999999999,1.90957148266057E-14));
#19287=CARTESIAN_POINT('Ctrl Pts',(-2.1650635094611,3.73333333333333,-1.24999999999999));
#19288=CARTESIAN_POINT('Ctrl Pts',(-1.44337567297407,3.79166666666666,-2.5));
#19289=CARTESIAN_POINT('Ctrl Pts',(-1.22495628946565E-14,3.84999999999999,
-2.5));
#19290=CARTESIAN_POINT('Ctrl Pts',(1.44337567297406,3.90833333333333,-2.5));
#19291=CARTESIAN_POINT('Ctrl Pts',(2.16506350946109,3.96666666666666,-1.25000000000001));
#19292=CARTESIAN_POINT('Ctrl Pts',(2.88675134594813,4.02499999999999,-9.19343891213498E-15));
#19293=CARTESIAN_POINT('Ctrl Pts',(2.16506350946111,4.08333333333333,1.24999999999998));
#19294=CARTESIAN_POINT('Ctrl Pts',(1.44337567297408,4.14166666666666,2.49999999999999));
#19295=CARTESIAN_POINT('Ctrl Pts',(-1.02907469966573E-13,4.2,2.5));
#19296=CARTESIAN_POINT('Origin',(-1.80160437084306E-13,4.2,2.15));
#19297=CARTESIAN_POINT('Ctrl Pts',(0.,0.35,2.15));
#19298=CARTESIAN_POINT('Ctrl Pts',(-1.2413030787577,0.408333333333333,2.15));
#19299=CARTESIAN_POINT('Ctrl Pts',(-1.86195461813654,0.466666666666667,
1.075));
#19300=CARTESIAN_POINT('Ctrl Pts',(-2.48260615751539,0.525,1.52015784217237E-16));
#19301=CARTESIAN_POINT('Ctrl Pts',(-1.86195461813654,0.583333333333333,
-1.075));
#19302=CARTESIAN_POINT('Ctrl Pts',(-1.2413030787577,0.641666666666666,-2.15));
#19303=CARTESIAN_POINT('Ctrl Pts',(-2.63299061816681E-16,0.699999999999999,
-2.15));
#19304=CARTESIAN_POINT('Ctrl Pts',(1.24130307875769,0.758333333333333,-2.15));
#19305=CARTESIAN_POINT('Ctrl Pts',(1.86195461813654,0.816666666666666,-1.075));
#19306=CARTESIAN_POINT('Ctrl Pts',(2.48260615751539,0.874999999999999,-4.5604735265171E-16));
#19307=CARTESIAN_POINT('Ctrl Pts',(1.86195461813654,0.933333333333332,1.075));
#19308=CARTESIAN_POINT('Ctrl Pts',(1.2413030787577,0.991666666666666,2.15));
#19309=CARTESIAN_POINT('Ctrl Pts',(0.,1.05,2.15));
#19310=CARTESIAN_POINT('Ctrl Pts',(-1.2413030787577,1.10833333333333,2.15));
#19311=CARTESIAN_POINT('Ctrl Pts',(-1.86195461813654,1.16666666666667,1.075));
#19312=CARTESIAN_POINT('Ctrl Pts',(-2.48260615751539,1.225,1.52015784217237E-16));
#19313=CARTESIAN_POINT('Ctrl Pts',(-1.86195461813654,1.28333333333333,-1.075));
#19314=CARTESIAN_POINT('Ctrl Pts',(-1.2413030787577,1.34166666666666,-2.15));
#19315=CARTESIAN_POINT('Ctrl Pts',(-2.63299061816681E-16,1.4,-2.15));
#19316=CARTESIAN_POINT('Ctrl Pts',(1.24130307875769,1.45833333333333,-2.15));
#19317=CARTESIAN_POINT('Ctrl Pts',(1.86195461813654,1.51666666666666,-1.075));
#19318=CARTESIAN_POINT('Ctrl Pts',(2.48260615751539,1.575,-4.5604735265171E-16));
#19319=CARTESIAN_POINT('Ctrl Pts',(1.86195461813654,1.63333333333333,1.075));
#19320=CARTESIAN_POINT('Ctrl Pts',(1.2413030787577,1.69166666666666,2.15));
#19321=CARTESIAN_POINT('Ctrl Pts',(0.,1.75,2.15));
#19322=CARTESIAN_POINT('Ctrl Pts',(-1.2413030787577,1.80833333333333,2.15));
#19323=CARTESIAN_POINT('Ctrl Pts',(-1.86195461813654,1.86666666666666,1.075));
#19324=CARTESIAN_POINT('Ctrl Pts',(-2.48260615751539,1.925,1.52015784217237E-16));
#19325=CARTESIAN_POINT('Ctrl Pts',(-1.86195461813654,1.98333333333333,-1.075));
#19326=CARTESIAN_POINT('Ctrl Pts',(-1.2413030787577,2.04166666666666,-2.15));
#19327=CARTESIAN_POINT('Ctrl Pts',(-2.63299061816681E-16,2.1,-2.15));
#19328=CARTESIAN_POINT('Ctrl Pts',(1.24130307875769,2.15833333333333,-2.15));
#19329=CARTESIAN_POINT('Ctrl Pts',(1.86195461813654,2.21666666666666,-1.075));
#19330=CARTESIAN_POINT('Ctrl Pts',(2.48260615751539,2.275,-4.5604735265171E-16));
#19331=CARTESIAN_POINT('Ctrl Pts',(1.86195461813654,2.33333333333333,1.075));
#19332=CARTESIAN_POINT('Ctrl Pts',(1.2413030787577,2.39166666666666,2.15));
#19333=CARTESIAN_POINT('Ctrl Pts',(0.,2.45,2.15));
#19334=CARTESIAN_POINT('Ctrl Pts',(-1.2413030787577,2.50833333333333,2.15));
#19335=CARTESIAN_POINT('Ctrl Pts',(-1.86195461813654,2.56666666666666,1.075));
#19336=CARTESIAN_POINT('Ctrl Pts',(-2.48260615751539,2.625,1.52015784217237E-16));
#19337=CARTESIAN_POINT('Ctrl Pts',(-1.86195461813654,2.68333333333333,-1.075));
#19338=CARTESIAN_POINT('Ctrl Pts',(-1.2413030787577,2.74166666666666,-2.15));
#19339=CARTESIAN_POINT('Ctrl Pts',(-2.63299061816681E-16,2.8,-2.15));
#19340=CARTESIAN_POINT('Ctrl Pts',(1.24130307875769,2.85833333333333,-2.15));
#19341=CARTESIAN_POINT('Ctrl Pts',(1.86195461813654,2.91666666666666,-1.075));
#19342=CARTESIAN_POINT('Ctrl Pts',(2.48260615751539,2.97499999999999,-4.5604735265171E-16));
#19343=CARTESIAN_POINT('Ctrl Pts',(1.86195461813654,3.03333333333333,1.075));
#19344=CARTESIAN_POINT('Ctrl Pts',(1.2413030787577,3.09166666666666,2.15));
#19345=CARTESIAN_POINT('Ctrl Pts',(0.,3.15,2.15));
#19346=CARTESIAN_POINT('Ctrl Pts',(-1.2413030787577,3.20833333333333,2.15));
#19347=CARTESIAN_POINT('Ctrl Pts',(-1.86195461813654,3.26666666666666,1.075));
#19348=CARTESIAN_POINT('Ctrl Pts',(-2.48260615751539,3.32499999999999,1.52015784217237E-16));
#19349=CARTESIAN_POINT('Ctrl Pts',(-1.86195461813654,3.38333333333333,-1.075));
#19350=CARTESIAN_POINT('Ctrl Pts',(-1.2413030787577,3.44166666666666,-2.15));
#19351=CARTESIAN_POINT('Ctrl Pts',(-2.63299061816681E-16,3.49999999999999,
-2.15));
#19352=CARTESIAN_POINT('Ctrl Pts',(1.24130307875769,3.55833333333333,-2.15));
#19353=CARTESIAN_POINT('Ctrl Pts',(1.86195461813654,3.61666666666666,-1.075));
#19354=CARTESIAN_POINT('Ctrl Pts',(2.48260615751539,3.67499999999999,-4.5604735265171E-16));
#19355=CARTESIAN_POINT('Ctrl Pts',(1.86195461813654,3.73333333333333,1.075));
#19356=CARTESIAN_POINT('Ctrl Pts',(1.2413030787577,3.79166666666666,2.15));
#19357=CARTESIAN_POINT('Ctrl Pts',(0.,3.84999999999999,2.15));
#19358=CARTESIAN_POINT('Ctrl Pts',(-1.2413030787577,3.90833333333333,2.15));
#19359=CARTESIAN_POINT('Ctrl Pts',(-1.86195461813654,3.96666666666666,1.075));
#19360=CARTESIAN_POINT('Ctrl Pts',(-2.48260615751539,4.02499999999999,1.52015784217237E-16));
#19361=CARTESIAN_POINT('Ctrl Pts',(-1.86195461813654,4.08333333333333,-1.075));
#19362=CARTESIAN_POINT('Ctrl Pts',(-1.2413030787577,4.14166666666666,-2.15));
#19363=CARTESIAN_POINT('Ctrl Pts',(-2.63299061816681E-16,4.19999999999999,
-2.15));
#19364=CARTESIAN_POINT('Ctrl Pts',(1.24130307875769,4.25833333333333,-2.15));
#19365=CARTESIAN_POINT('Ctrl Pts',(1.86195461813654,4.31666666666666,-1.075));
#19366=CARTESIAN_POINT('Ctrl Pts',(2.48260615751539,4.37499999999999,-4.5604735265171E-16));
#19367=CARTESIAN_POINT('Ctrl Pts',(1.86195461813654,4.43333333333333,1.075));
#19368=CARTESIAN_POINT('Ctrl Pts',(1.2413030787577,4.49166666666666,2.15));
#19369=CARTESIAN_POINT('Ctrl Pts',(0.,4.54999999999999,2.15));
#19370=CARTESIAN_POINT('Ctrl Pts',(0.,0.35,2.35502525316942));
#19371=CARTESIAN_POINT('Ctrl Pts',(-1.35967446386573,0.408333333333333,
2.35502525316942));
#19372=CARTESIAN_POINT('Ctrl Pts',(-2.03951169579859,0.466666666666666,
1.17751262658471));
#19373=CARTESIAN_POINT('Ctrl Pts',(-2.71934892773146,0.525,1.66512098005556E-16));
#19374=CARTESIAN_POINT('Ctrl Pts',(-2.03951169579859,0.583333333333333,
-1.17751262658471));
#19375=CARTESIAN_POINT('Ctrl Pts',(-1.35967446386573,0.641666666666666,
-2.35502525316942));
#19376=CARTESIAN_POINT('Ctrl Pts',(-2.88407413820511E-16,0.699999999999999,
-2.35502525316942));
#19377=CARTESIAN_POINT('Ctrl Pts',(1.35967446386573,0.758333333333333,-2.35502525316942));
#19378=CARTESIAN_POINT('Ctrl Pts',(2.03951169579859,0.816666666666666,-1.17751262658471));
#19379=CARTESIAN_POINT('Ctrl Pts',(2.71934892773146,0.874999999999999,-4.99536294016668E-16));
#19380=CARTESIAN_POINT('Ctrl Pts',(2.03951169579859,0.933333333333332,1.17751262658471));
#19381=CARTESIAN_POINT('Ctrl Pts',(1.35967446386573,0.991666666666665,2.35502525316942));
#19382=CARTESIAN_POINT('Ctrl Pts',(0.,1.05,2.35502525316942));
#19383=CARTESIAN_POINT('Ctrl Pts',(-1.35967446386573,1.10833333333333,2.35502525316942));
#19384=CARTESIAN_POINT('Ctrl Pts',(-2.03951169579859,1.16666666666666,1.17751262658471));
#19385=CARTESIAN_POINT('Ctrl Pts',(-2.71934892773146,1.225,1.66512098005556E-16));
#19386=CARTESIAN_POINT('Ctrl Pts',(-2.03951169579859,1.28333333333333,-1.17751262658471));
#19387=CARTESIAN_POINT('Ctrl Pts',(-1.35967446386573,1.34166666666667,-2.35502525316942));
#19388=CARTESIAN_POINT('Ctrl Pts',(-2.88407413820511E-16,1.4,-2.35502525316942));
#19389=CARTESIAN_POINT('Ctrl Pts',(1.35967446386573,1.45833333333333,-2.35502525316942));
#19390=CARTESIAN_POINT('Ctrl Pts',(2.03951169579859,1.51666666666666,-1.17751262658471));
#19391=CARTESIAN_POINT('Ctrl Pts',(2.71934892773146,1.575,-4.99536294016668E-16));
#19392=CARTESIAN_POINT('Ctrl Pts',(2.03951169579859,1.63333333333333,1.17751262658471));
#19393=CARTESIAN_POINT('Ctrl Pts',(1.35967446386573,1.69166666666666,2.35502525316942));
#19394=CARTESIAN_POINT('Ctrl Pts',(0.,1.75,2.35502525316942));
#19395=CARTESIAN_POINT('Ctrl Pts',(-1.35967446386573,1.80833333333333,2.35502525316942));
#19396=CARTESIAN_POINT('Ctrl Pts',(-2.03951169579859,1.86666666666666,1.17751262658471));
#19397=CARTESIAN_POINT('Ctrl Pts',(-2.71934892773146,1.925,1.66512098005556E-16));
#19398=CARTESIAN_POINT('Ctrl Pts',(-2.03951169579859,1.98333333333333,-1.17751262658471));
#19399=CARTESIAN_POINT('Ctrl Pts',(-1.35967446386573,2.04166666666666,-2.35502525316942));
#19400=CARTESIAN_POINT('Ctrl Pts',(-2.88407413820511E-16,2.1,-2.35502525316942));
#19401=CARTESIAN_POINT('Ctrl Pts',(1.35967446386573,2.15833333333333,-2.35502525316942));
#19402=CARTESIAN_POINT('Ctrl Pts',(2.03951169579859,2.21666666666666,-1.17751262658471));
#19403=CARTESIAN_POINT('Ctrl Pts',(2.71934892773146,2.275,-4.99536294016668E-16));
#19404=CARTESIAN_POINT('Ctrl Pts',(2.03951169579859,2.33333333333333,1.17751262658471));
#19405=CARTESIAN_POINT('Ctrl Pts',(1.35967446386573,2.39166666666666,2.35502525316942));
#19406=CARTESIAN_POINT('Ctrl Pts',(0.,2.45,2.35502525316942));
#19407=CARTESIAN_POINT('Ctrl Pts',(-1.35967446386573,2.50833333333333,2.35502525316942));
#19408=CARTESIAN_POINT('Ctrl Pts',(-2.03951169579859,2.56666666666666,1.17751262658471));
#19409=CARTESIAN_POINT('Ctrl Pts',(-2.71934892773146,2.62499999999999,1.66512098005556E-16));
#19410=CARTESIAN_POINT('Ctrl Pts',(-2.03951169579859,2.68333333333333,-1.17751262658471));
#19411=CARTESIAN_POINT('Ctrl Pts',(-1.35967446386573,2.74166666666666,-2.35502525316942));
#19412=CARTESIAN_POINT('Ctrl Pts',(-2.88407413820511E-16,2.8,-2.35502525316942));
#19413=CARTESIAN_POINT('Ctrl Pts',(1.35967446386573,2.85833333333333,-2.35502525316942));
#19414=CARTESIAN_POINT('Ctrl Pts',(2.03951169579859,2.91666666666666,-1.17751262658471));
#19415=CARTESIAN_POINT('Ctrl Pts',(2.71934892773146,2.97499999999999,-4.99536294016668E-16));
#19416=CARTESIAN_POINT('Ctrl Pts',(2.03951169579859,3.03333333333333,1.17751262658471));
#19417=CARTESIAN_POINT('Ctrl Pts',(1.35967446386573,3.09166666666666,2.35502525316942));
#19418=CARTESIAN_POINT('Ctrl Pts',(0.,3.14999999999999,2.35502525316942));
#19419=CARTESIAN_POINT('Ctrl Pts',(-1.35967446386573,3.20833333333333,2.35502525316942));
#19420=CARTESIAN_POINT('Ctrl Pts',(-2.03951169579859,3.26666666666666,1.17751262658471));
#19421=CARTESIAN_POINT('Ctrl Pts',(-2.71934892773146,3.32499999999999,1.66512098005556E-16));
#19422=CARTESIAN_POINT('Ctrl Pts',(-2.03951169579859,3.38333333333333,-1.17751262658471));
#19423=CARTESIAN_POINT('Ctrl Pts',(-1.35967446386573,3.44166666666666,-2.35502525316942));
#19424=CARTESIAN_POINT('Ctrl Pts',(-2.88407413820511E-16,3.49999999999999,
-2.35502525316942));
#19425=CARTESIAN_POINT('Ctrl Pts',(1.35967446386573,3.55833333333333,-2.35502525316942));
#19426=CARTESIAN_POINT('Ctrl Pts',(2.03951169579859,3.61666666666666,-1.17751262658471));
#19427=CARTESIAN_POINT('Ctrl Pts',(2.71934892773146,3.67499999999999,-4.99536294016668E-16));
#19428=CARTESIAN_POINT('Ctrl Pts',(2.03951169579859,3.73333333333333,1.17751262658471));
#19429=CARTESIAN_POINT('Ctrl Pts',(1.35967446386573,3.79166666666666,2.35502525316942));
#19430=CARTESIAN_POINT('Ctrl Pts',(0.,3.84999999999999,2.35502525316942));
#19431=CARTESIAN_POINT('Ctrl Pts',(-1.35967446386573,3.90833333333333,2.35502525316942));
#19432=CARTESIAN_POINT('Ctrl Pts',(-2.03951169579859,3.96666666666666,1.17751262658471));
#19433=CARTESIAN_POINT('Ctrl Pts',(-2.71934892773146,4.02499999999999,1.66512098005556E-16));
#19434=CARTESIAN_POINT('Ctrl Pts',(-2.03951169579859,4.08333333333333,-1.17751262658471));
#19435=CARTESIAN_POINT('Ctrl Pts',(-1.35967446386573,4.14166666666666,-2.35502525316942));
#19436=CARTESIAN_POINT('Ctrl Pts',(-2.88407413820511E-16,4.19999999999999,
-2.35502525316942));
#19437=CARTESIAN_POINT('Ctrl Pts',(1.35967446386573,4.25833333333332,-2.35502525316942));
#19438=CARTESIAN_POINT('Ctrl Pts',(2.03951169579859,4.31666666666666,-1.17751262658471));
#19439=CARTESIAN_POINT('Ctrl Pts',(2.71934892773146,4.37499999999999,-4.99536294016668E-16));
#19440=CARTESIAN_POINT('Ctrl Pts',(2.03951169579859,4.43333333333332,1.17751262658471));
#19441=CARTESIAN_POINT('Ctrl Pts',(1.35967446386573,4.49166666666666,2.35502525316942));
#19442=CARTESIAN_POINT('Ctrl Pts',(0.,4.54999999999999,2.35502525316942));
#19443=CARTESIAN_POINT('Ctrl Pts',(0.,0.205025253169417,2.5));
#19444=CARTESIAN_POINT('Ctrl Pts',(-1.44337567297406,0.26335858650275,2.5));
#19445=CARTESIAN_POINT('Ctrl Pts',(-2.1650635094611,0.321691919836083,1.25));
#19446=CARTESIAN_POINT('Ctrl Pts',(-2.88675134594813,0.380025253169416,
1.76762539787484E-16));
#19447=CARTESIAN_POINT('Ctrl Pts',(-2.1650635094611,0.43835858650275,-1.25));
#19448=CARTESIAN_POINT('Ctrl Pts',(-1.44337567297407,0.496691919836083,
-2.5));
#19449=CARTESIAN_POINT('Ctrl Pts',(-3.06161699786838E-16,0.555025253169416,
-2.5));
#19450=CARTESIAN_POINT('Ctrl Pts',(1.44337567297406,0.613358586502749,-2.5));
#19451=CARTESIAN_POINT('Ctrl Pts',(2.1650635094611,0.671691919836083,-1.25));
#19452=CARTESIAN_POINT('Ctrl Pts',(2.88675134594813,0.730025253169416,-5.30287619362453E-16));
#19453=CARTESIAN_POINT('Ctrl Pts',(2.1650635094611,0.788358586502749,1.25));
#19454=CARTESIAN_POINT('Ctrl Pts',(1.44337567297407,0.846691919836082,2.5));
#19455=CARTESIAN_POINT('Ctrl Pts',(0.,0.905025253169415,2.5));
#19456=CARTESIAN_POINT('Ctrl Pts',(-1.44337567297406,0.963358586502749,
2.5));
#19457=CARTESIAN_POINT('Ctrl Pts',(-2.1650635094611,1.02169191983608,1.25));
#19458=CARTESIAN_POINT('Ctrl Pts',(-2.88675134594813,1.08002525316942,1.76762539787484E-16));
#19459=CARTESIAN_POINT('Ctrl Pts',(-2.1650635094611,1.13835858650275,-1.25));
#19460=CARTESIAN_POINT('Ctrl Pts',(-1.44337567297407,1.19669191983608,-2.5));
#19461=CARTESIAN_POINT('Ctrl Pts',(-3.06161699786838E-16,1.25502525316941,
-2.5));
#19462=CARTESIAN_POINT('Ctrl Pts',(1.44337567297406,1.31335858650275,-2.5));
#19463=CARTESIAN_POINT('Ctrl Pts',(2.1650635094611,1.37169191983608,-1.25));
#19464=CARTESIAN_POINT('Ctrl Pts',(2.88675134594813,1.43002525316941,-5.30287619362453E-16));
#19465=CARTESIAN_POINT('Ctrl Pts',(2.1650635094611,1.48835858650275,1.25));
#19466=CARTESIAN_POINT('Ctrl Pts',(1.44337567297407,1.54669191983608,2.5));
#19467=CARTESIAN_POINT('Ctrl Pts',(0.,1.60502525316941,2.5));
#19468=CARTESIAN_POINT('Ctrl Pts',(-1.44337567297406,1.66335858650275,2.5));
#19469=CARTESIAN_POINT('Ctrl Pts',(-2.1650635094611,1.72169191983608,1.25));
#19470=CARTESIAN_POINT('Ctrl Pts',(-2.88675134594813,1.78002525316941,1.76762539787484E-16));
#19471=CARTESIAN_POINT('Ctrl Pts',(-2.1650635094611,1.83835858650275,-1.25));
#19472=CARTESIAN_POINT('Ctrl Pts',(-1.44337567297407,1.89669191983608,-2.5));
#19473=CARTESIAN_POINT('Ctrl Pts',(-3.06161699786838E-16,1.95502525316941,
-2.5));
#19474=CARTESIAN_POINT('Ctrl Pts',(1.44337567297406,2.01335858650275,-2.5));
#19475=CARTESIAN_POINT('Ctrl Pts',(2.1650635094611,2.07169191983608,-1.25));
#19476=CARTESIAN_POINT('Ctrl Pts',(2.88675134594813,2.13002525316941,-5.30287619362453E-16));
#19477=CARTESIAN_POINT('Ctrl Pts',(2.1650635094611,2.18835858650275,1.25));
#19478=CARTESIAN_POINT('Ctrl Pts',(1.44337567297407,2.24669191983608,2.5));
#19479=CARTESIAN_POINT('Ctrl Pts',(0.,2.30502525316941,2.5));
#19480=CARTESIAN_POINT('Ctrl Pts',(-1.44337567297406,2.36335858650275,2.5));
#19481=CARTESIAN_POINT('Ctrl Pts',(-2.1650635094611,2.42169191983608,1.25));
#19482=CARTESIAN_POINT('Ctrl Pts',(-2.88675134594813,2.48002525316941,1.76762539787484E-16));
#19483=CARTESIAN_POINT('Ctrl Pts',(-2.1650635094611,2.53835858650275,-1.25));
#19484=CARTESIAN_POINT('Ctrl Pts',(-1.44337567297407,2.59669191983608,-2.5));
#19485=CARTESIAN_POINT('Ctrl Pts',(-3.06161699786838E-16,2.65502525316941,
-2.5));
#19486=CARTESIAN_POINT('Ctrl Pts',(1.44337567297406,2.71335858650274,-2.5));
#19487=CARTESIAN_POINT('Ctrl Pts',(2.1650635094611,2.77169191983608,-1.25));
#19488=CARTESIAN_POINT('Ctrl Pts',(2.88675134594813,2.83002525316941,-5.30287619362453E-16));
#19489=CARTESIAN_POINT('Ctrl Pts',(2.1650635094611,2.88835858650274,1.25));
#19490=CARTESIAN_POINT('Ctrl Pts',(1.44337567297407,2.94669191983608,2.5));
#19491=CARTESIAN_POINT('Ctrl Pts',(0.,3.00502525316941,2.5));
#19492=CARTESIAN_POINT('Ctrl Pts',(-1.44337567297406,3.06335858650274,2.5));
#19493=CARTESIAN_POINT('Ctrl Pts',(-2.1650635094611,3.12169191983608,1.25));
#19494=CARTESIAN_POINT('Ctrl Pts',(-2.88675134594813,3.18002525316941,1.76762539787484E-16));
#19495=CARTESIAN_POINT('Ctrl Pts',(-2.1650635094611,3.23835858650274,-1.25));
#19496=CARTESIAN_POINT('Ctrl Pts',(-1.44337567297407,3.29669191983608,-2.5));
#19497=CARTESIAN_POINT('Ctrl Pts',(-3.06161699786838E-16,3.35502525316941,
-2.5));
#19498=CARTESIAN_POINT('Ctrl Pts',(1.44337567297406,3.41335858650274,-2.5));
#19499=CARTESIAN_POINT('Ctrl Pts',(2.1650635094611,3.47169191983608,-1.25));
#19500=CARTESIAN_POINT('Ctrl Pts',(2.88675134594813,3.53002525316941,-5.30287619362453E-16));
#19501=CARTESIAN_POINT('Ctrl Pts',(2.1650635094611,3.58835858650274,1.25));
#19502=CARTESIAN_POINT('Ctrl Pts',(1.44337567297407,3.64669191983608,2.5));
#19503=CARTESIAN_POINT('Ctrl Pts',(0.,3.70502525316941,2.5));
#19504=CARTESIAN_POINT('Ctrl Pts',(-1.44337567297406,3.76335858650274,2.5));
#19505=CARTESIAN_POINT('Ctrl Pts',(-2.1650635094611,3.82169191983608,1.25));
#19506=CARTESIAN_POINT('Ctrl Pts',(-2.88675134594813,3.88002525316941,1.76762539787484E-16));
#19507=CARTESIAN_POINT('Ctrl Pts',(-2.1650635094611,3.93835858650274,-1.25));
#19508=CARTESIAN_POINT('Ctrl Pts',(-1.44337567297407,3.99669191983608,-2.5));
#19509=CARTESIAN_POINT('Ctrl Pts',(-3.06161699786838E-16,4.05502525316941,
-2.5));
#19510=CARTESIAN_POINT('Ctrl Pts',(1.44337567297406,4.11335858650274,-2.5));
#19511=CARTESIAN_POINT('Ctrl Pts',(2.1650635094611,4.17169191983608,-1.25));
#19512=CARTESIAN_POINT('Ctrl Pts',(2.88675134594813,4.23002525316941,-5.30287619362453E-16));
#19513=CARTESIAN_POINT('Ctrl Pts',(2.1650635094611,4.28835858650274,1.25));
#19514=CARTESIAN_POINT('Ctrl Pts',(1.44337567297407,4.34669191983608,2.5));
#19515=CARTESIAN_POINT('Ctrl Pts',(0.,4.40502525316941,2.5));
#19516=CARTESIAN_POINT('Ctrl Pts',(0.,4.28626379701574E-17,2.5));
#19517=CARTESIAN_POINT('Ctrl Pts',(-1.44337567297406,0.0583333333333333,
2.5));
#19518=CARTESIAN_POINT('Ctrl Pts',(-2.1650635094611,0.116666666666666,1.25));
#19519=CARTESIAN_POINT('Ctrl Pts',(-2.88675134594813,0.175,1.76762539787484E-16));
#19520=CARTESIAN_POINT('Ctrl Pts',(-2.1650635094611,0.233333333333333,-1.25));
#19521=CARTESIAN_POINT('Ctrl Pts',(-1.44337567297407,0.291666666666666,
-2.5));
#19522=CARTESIAN_POINT('Ctrl Pts',(-3.06161699786838E-16,0.349999999999999,
-2.5));
#19523=CARTESIAN_POINT('Ctrl Pts',(1.44337567297406,0.408333333333333,-2.5));
#19524=CARTESIAN_POINT('Ctrl Pts',(2.1650635094611,0.466666666666666,-1.25));
#19525=CARTESIAN_POINT('Ctrl Pts',(2.88675134594813,0.524999999999999,-5.30287619362453E-16));
#19526=CARTESIAN_POINT('Ctrl Pts',(2.1650635094611,0.583333333333332,1.25));
#19527=CARTESIAN_POINT('Ctrl Pts',(1.44337567297407,0.641666666666665,2.5));
#19528=CARTESIAN_POINT('Ctrl Pts',(0.,0.699999999999999,2.5));
#19529=CARTESIAN_POINT('Ctrl Pts',(-1.44337567297406,0.758333333333332,
2.5));
#19530=CARTESIAN_POINT('Ctrl Pts',(-2.1650635094611,0.816666666666665,1.25));
#19531=CARTESIAN_POINT('Ctrl Pts',(-2.88675134594813,0.874999999999998,
1.76762539787484E-16));
#19532=CARTESIAN_POINT('Ctrl Pts',(-2.1650635094611,0.933333333333332,-1.25));
#19533=CARTESIAN_POINT('Ctrl Pts',(-1.44337567297407,0.991666666666665,
-2.5));
#19534=CARTESIAN_POINT('Ctrl Pts',(-3.06161699786838E-16,1.05,-2.5));
#19535=CARTESIAN_POINT('Ctrl Pts',(1.44337567297406,1.10833333333333,-2.5));
#19536=CARTESIAN_POINT('Ctrl Pts',(2.1650635094611,1.16666666666666,-1.25));
#19537=CARTESIAN_POINT('Ctrl Pts',(2.88675134594813,1.225,-5.30287619362453E-16));
#19538=CARTESIAN_POINT('Ctrl Pts',(2.1650635094611,1.28333333333333,1.25));
#19539=CARTESIAN_POINT('Ctrl Pts',(1.44337567297407,1.34166666666666,2.5));
#19540=CARTESIAN_POINT('Ctrl Pts',(0.,1.4,2.5));
#19541=CARTESIAN_POINT('Ctrl Pts',(-1.44337567297406,1.45833333333333,2.5));
#19542=CARTESIAN_POINT('Ctrl Pts',(-2.1650635094611,1.51666666666666,1.25));
#19543=CARTESIAN_POINT('Ctrl Pts',(-2.88675134594813,1.575,1.76762539787484E-16));
#19544=CARTESIAN_POINT('Ctrl Pts',(-2.1650635094611,1.63333333333333,-1.25));
#19545=CARTESIAN_POINT('Ctrl Pts',(-1.44337567297407,1.69166666666666,-2.5));
#19546=CARTESIAN_POINT('Ctrl Pts',(-3.06161699786838E-16,1.75,-2.5));
#19547=CARTESIAN_POINT('Ctrl Pts',(1.44337567297406,1.80833333333333,-2.5));
#19548=CARTESIAN_POINT('Ctrl Pts',(2.1650635094611,1.86666666666666,-1.25));
#19549=CARTESIAN_POINT('Ctrl Pts',(2.88675134594813,1.925,-5.30287619362453E-16));
#19550=CARTESIAN_POINT('Ctrl Pts',(2.1650635094611,1.98333333333333,1.25));
#19551=CARTESIAN_POINT('Ctrl Pts',(1.44337567297407,2.04166666666666,2.5));
#19552=CARTESIAN_POINT('Ctrl Pts',(0.,2.1,2.5));
#19553=CARTESIAN_POINT('Ctrl Pts',(-1.44337567297406,2.15833333333333,2.5));
#19554=CARTESIAN_POINT('Ctrl Pts',(-2.1650635094611,2.21666666666666,1.25));
#19555=CARTESIAN_POINT('Ctrl Pts',(-2.88675134594813,2.275,1.76762539787484E-16));
#19556=CARTESIAN_POINT('Ctrl Pts',(-2.1650635094611,2.33333333333333,-1.25));
#19557=CARTESIAN_POINT('Ctrl Pts',(-1.44337567297407,2.39166666666666,-2.5));
#19558=CARTESIAN_POINT('Ctrl Pts',(-3.06161699786838E-16,2.45,-2.5));
#19559=CARTESIAN_POINT('Ctrl Pts',(1.44337567297406,2.50833333333333,-2.5));
#19560=CARTESIAN_POINT('Ctrl Pts',(2.1650635094611,2.56666666666666,-1.25));
#19561=CARTESIAN_POINT('Ctrl Pts',(2.88675134594813,2.62499999999999,-5.30287619362453E-16));
#19562=CARTESIAN_POINT('Ctrl Pts',(2.1650635094611,2.68333333333333,1.25));
#19563=CARTESIAN_POINT('Ctrl Pts',(1.44337567297407,2.74166666666666,2.5));
#19564=CARTESIAN_POINT('Ctrl Pts',(0.,2.79999999999999,2.5));
#19565=CARTESIAN_POINT('Ctrl Pts',(-1.44337567297406,2.85833333333333,2.5));
#19566=CARTESIAN_POINT('Ctrl Pts',(-2.1650635094611,2.91666666666666,1.25));
#19567=CARTESIAN_POINT('Ctrl Pts',(-2.88675134594813,2.97499999999999,1.76762539787484E-16));
#19568=CARTESIAN_POINT('Ctrl Pts',(-2.1650635094611,3.03333333333333,-1.25));
#19569=CARTESIAN_POINT('Ctrl Pts',(-1.44337567297407,3.09166666666666,-2.5));
#19570=CARTESIAN_POINT('Ctrl Pts',(-3.06161699786838E-16,3.14999999999999,
-2.5));
#19571=CARTESIAN_POINT('Ctrl Pts',(1.44337567297406,3.20833333333333,-2.5));
#19572=CARTESIAN_POINT('Ctrl Pts',(2.1650635094611,3.26666666666666,-1.25));
#19573=CARTESIAN_POINT('Ctrl Pts',(2.88675134594813,3.32499999999999,-5.30287619362453E-16));
#19574=CARTESIAN_POINT('Ctrl Pts',(2.1650635094611,3.38333333333333,1.25));
#19575=CARTESIAN_POINT('Ctrl Pts',(1.44337567297407,3.44166666666666,2.5));
#19576=CARTESIAN_POINT('Ctrl Pts',(0.,3.49999999999999,2.5));
#19577=CARTESIAN_POINT('Ctrl Pts',(-1.44337567297406,3.55833333333333,2.5));
#19578=CARTESIAN_POINT('Ctrl Pts',(-2.1650635094611,3.61666666666666,1.25));
#19579=CARTESIAN_POINT('Ctrl Pts',(-2.88675134594813,3.67499999999999,1.76762539787484E-16));
#19580=CARTESIAN_POINT('Ctrl Pts',(-2.1650635094611,3.73333333333333,-1.25));
#19581=CARTESIAN_POINT('Ctrl Pts',(-1.44337567297407,3.79166666666666,-2.5));
#19582=CARTESIAN_POINT('Ctrl Pts',(-3.06161699786838E-16,3.84999999999999,
-2.5));
#19583=CARTESIAN_POINT('Ctrl Pts',(1.44337567297406,3.90833333333333,-2.5));
#19584=CARTESIAN_POINT('Ctrl Pts',(2.1650635094611,3.96666666666666,-1.25));
#19585=CARTESIAN_POINT('Ctrl Pts',(2.88675134594813,4.02499999999999,-5.30287619362453E-16));
#19586=CARTESIAN_POINT('Ctrl Pts',(2.1650635094611,4.08333333333333,1.25));
#19587=CARTESIAN_POINT('Ctrl Pts',(1.44337567297407,4.14166666666666,2.5));
#19588=CARTESIAN_POINT('Ctrl Pts',(0.,4.19999999999999,2.5));
#19589=CARTESIAN_POINT('Origin',(0.,0.,2.15));
#19590=CARTESIAN_POINT('Origin',(-1.80160437084306E-13,4.2,2.15));
#19591=CARTESIAN_POINT('Origin',(-1.80160437084306E-13,4.2,2.15));
#19592=CARTESIAN_POINT('Origin',(0.,0.,2.15));
#19593=CARTESIAN_POINT('',(0.,0.,0.));
#19594=CARTESIAN_POINT('Ctrl Pts',(0.,0.,1.8));
#19595=CARTESIAN_POINT('Ctrl Pts',(-1.03923048454133,0.0583333333333332,
1.8));
#19596=CARTESIAN_POINT('Ctrl Pts',(-1.55884572681199,0.116666666666666,
0.9));
#19597=CARTESIAN_POINT('Ctrl Pts',(-2.07846096908265,0.175,1.27269028646989E-16));
#19598=CARTESIAN_POINT('Ctrl Pts',(-1.55884572681199,0.233333333333333,
-0.9));
#19599=CARTESIAN_POINT('Ctrl Pts',(-1.03923048454133,0.291666666666666,
-1.8));
#19600=CARTESIAN_POINT('Ctrl Pts',(-2.20436423846524E-16,0.349999999999999,
-1.8));
#19601=CARTESIAN_POINT('Ctrl Pts',(1.03923048454133,0.408333333333333,-1.8));
#19602=CARTESIAN_POINT('Ctrl Pts',(1.55884572681199,0.466666666666666,-0.900000000000001));
#19603=CARTESIAN_POINT('Ctrl Pts',(2.07846096908265,0.524999999999999,-3.81807085940967E-16));
#19604=CARTESIAN_POINT('Ctrl Pts',(1.55884572681199,0.583333333333332,0.899999999999999));
#19605=CARTESIAN_POINT('Ctrl Pts',(1.03923048454133,0.641666666666665,1.8));
#19606=CARTESIAN_POINT('Ctrl Pts',(0.,0.699999999999999,1.8));
#19607=CARTESIAN_POINT('Ctrl Pts',(-1.03923048454133,0.758333333333332,
1.8));
#19608=CARTESIAN_POINT('Ctrl Pts',(-1.55884572681199,0.816666666666665,
0.9));
#19609=CARTESIAN_POINT('Ctrl Pts',(-2.07846096908265,0.874999999999998,
1.27269028646989E-16));
#19610=CARTESIAN_POINT('Ctrl Pts',(-1.55884572681199,0.933333333333332,
-0.9));
#19611=CARTESIAN_POINT('Ctrl Pts',(-1.03923048454133,0.991666666666665,
-1.8));
#19612=CARTESIAN_POINT('Ctrl Pts',(-2.20436423846524E-16,1.05,-1.8));
#19613=CARTESIAN_POINT('Ctrl Pts',(1.03923048454133,1.10833333333333,-1.8));
#19614=CARTESIAN_POINT('Ctrl Pts',(1.55884572681199,1.16666666666666,-0.900000000000001));
#19615=CARTESIAN_POINT('Ctrl Pts',(2.07846096908265,1.225,-3.81807085940967E-16));
#19616=CARTESIAN_POINT('Ctrl Pts',(1.55884572681199,1.28333333333333,0.899999999999999));
#19617=CARTESIAN_POINT('Ctrl Pts',(1.03923048454133,1.34166666666666,1.8));
#19618=CARTESIAN_POINT('Ctrl Pts',(0.,1.4,1.8));
#19619=CARTESIAN_POINT('Ctrl Pts',(-1.03923048454133,1.45833333333333,1.8));
#19620=CARTESIAN_POINT('Ctrl Pts',(-1.55884572681199,1.51666666666666,0.9));
#19621=CARTESIAN_POINT('Ctrl Pts',(-2.07846096908265,1.575,1.27269028646989E-16));
#19622=CARTESIAN_POINT('Ctrl Pts',(-1.55884572681199,1.63333333333333,-0.9));
#19623=CARTESIAN_POINT('Ctrl Pts',(-1.03923048454133,1.69166666666666,-1.8));
#19624=CARTESIAN_POINT('Ctrl Pts',(-2.20436423846524E-16,1.75,-1.8));
#19625=CARTESIAN_POINT('Ctrl Pts',(1.03923048454133,1.80833333333333,-1.8));
#19626=CARTESIAN_POINT('Ctrl Pts',(1.55884572681199,1.86666666666666,-0.900000000000001));
#19627=CARTESIAN_POINT('Ctrl Pts',(2.07846096908265,1.925,-3.81807085940967E-16));
#19628=CARTESIAN_POINT('Ctrl Pts',(1.55884572681199,1.98333333333333,0.899999999999999));
#19629=CARTESIAN_POINT('Ctrl Pts',(1.03923048454133,2.04166666666666,1.8));
#19630=CARTESIAN_POINT('Ctrl Pts',(0.,2.1,1.8));
#19631=CARTESIAN_POINT('Ctrl Pts',(-1.03923048454133,2.15833333333333,1.8));
#19632=CARTESIAN_POINT('Ctrl Pts',(-1.55884572681199,2.21666666666666,0.9));
#19633=CARTESIAN_POINT('Ctrl Pts',(-2.07846096908265,2.275,1.27269028646989E-16));
#19634=CARTESIAN_POINT('Ctrl Pts',(-1.55884572681199,2.33333333333333,-0.9));
#19635=CARTESIAN_POINT('Ctrl Pts',(-1.03923048454133,2.39166666666666,-1.8));
#19636=CARTESIAN_POINT('Ctrl Pts',(-2.20436423846524E-16,2.45,-1.8));
#19637=CARTESIAN_POINT('Ctrl Pts',(1.03923048454133,2.50833333333333,-1.8));
#19638=CARTESIAN_POINT('Ctrl Pts',(1.55884572681199,2.56666666666666,-0.900000000000001));
#19639=CARTESIAN_POINT('Ctrl Pts',(2.07846096908265,2.62499999999999,-3.81807085940967E-16));
#19640=CARTESIAN_POINT('Ctrl Pts',(1.55884572681199,2.68333333333333,0.899999999999999));
#19641=CARTESIAN_POINT('Ctrl Pts',(1.03923048454133,2.74166666666666,1.8));
#19642=CARTESIAN_POINT('Ctrl Pts',(0.,2.79999999999999,1.8));
#19643=CARTESIAN_POINT('Ctrl Pts',(-1.03923048454133,2.85833333333333,1.8));
#19644=CARTESIAN_POINT('Ctrl Pts',(-1.55884572681199,2.91666666666666,0.9));
#19645=CARTESIAN_POINT('Ctrl Pts',(-2.07846096908265,2.97499999999999,1.27269028646989E-16));
#19646=CARTESIAN_POINT('Ctrl Pts',(-1.55884572681199,3.03333333333333,-0.9));
#19647=CARTESIAN_POINT('Ctrl Pts',(-1.03923048454133,3.09166666666666,-1.8));
#19648=CARTESIAN_POINT('Ctrl Pts',(-2.20436423846524E-16,3.14999999999999,
-1.8));
#19649=CARTESIAN_POINT('Ctrl Pts',(1.03923048454133,3.20833333333333,-1.8));
#19650=CARTESIAN_POINT('Ctrl Pts',(1.55884572681199,3.26666666666666,-0.900000000000001));
#19651=CARTESIAN_POINT('Ctrl Pts',(2.07846096908265,3.32499999999999,-3.81807085940967E-16));
#19652=CARTESIAN_POINT('Ctrl Pts',(1.55884572681199,3.38333333333333,0.899999999999999));
#19653=CARTESIAN_POINT('Ctrl Pts',(1.03923048454133,3.44166666666666,1.8));
#19654=CARTESIAN_POINT('Ctrl Pts',(0.,3.49999999999999,1.8));
#19655=CARTESIAN_POINT('Ctrl Pts',(-1.03923048454133,3.55833333333333,1.8));
#19656=CARTESIAN_POINT('Ctrl Pts',(-1.55884572681199,3.61666666666666,0.9));
#19657=CARTESIAN_POINT('Ctrl Pts',(-2.07846096908265,3.67499999999999,1.27269028646989E-16));
#19658=CARTESIAN_POINT('Ctrl Pts',(-1.55884572681199,3.73333333333333,-0.9));
#19659=CARTESIAN_POINT('Ctrl Pts',(-1.03923048454133,3.79166666666666,-1.8));
#19660=CARTESIAN_POINT('Ctrl Pts',(-2.20436423846524E-16,3.84999999999999,
-1.8));
#19661=CARTESIAN_POINT('Ctrl Pts',(1.03923048454133,3.90833333333333,-1.8));
#19662=CARTESIAN_POINT('Ctrl Pts',(1.55884572681199,3.96666666666666,-0.900000000000001));
#19663=CARTESIAN_POINT('Ctrl Pts',(2.07846096908265,4.02499999999999,-3.81807085940967E-16));
#19664=CARTESIAN_POINT('Ctrl Pts',(1.55884572681199,4.08333333333333,0.899999999999999));
#19665=CARTESIAN_POINT('Ctrl Pts',(1.03923048454133,4.14166666666666,1.8));
#19666=CARTESIAN_POINT('Ctrl Pts',(0.,4.19999999999999,1.8));
#19667=CARTESIAN_POINT('Ctrl Pts',(0.,0.205025253169417,1.8));
#19668=CARTESIAN_POINT('Ctrl Pts',(-1.03923048454133,0.26335858650275,1.8));
#19669=CARTESIAN_POINT('Ctrl Pts',(-1.55884572681199,0.321691919836083,
0.9));
#19670=CARTESIAN_POINT('Ctrl Pts',(-2.07846096908265,0.380025253169416,
1.27269028646989E-16));
#19671=CARTESIAN_POINT('Ctrl Pts',(-1.55884572681199,0.43835858650275,-0.9));
#19672=CARTESIAN_POINT('Ctrl Pts',(-1.03923048454133,0.496691919836083,
-1.8));
#19673=CARTESIAN_POINT('Ctrl Pts',(-2.20436423846524E-16,0.555025253169416,
-1.8));
#19674=CARTESIAN_POINT('Ctrl Pts',(1.03923048454133,0.613358586502749,-1.8));
#19675=CARTESIAN_POINT('Ctrl Pts',(1.55884572681199,0.671691919836083,-0.900000000000001));
#19676=CARTESIAN_POINT('Ctrl Pts',(2.07846096908265,0.730025253169416,-3.81807085940967E-16));
#19677=CARTESIAN_POINT('Ctrl Pts',(1.55884572681199,0.788358586502749,0.899999999999999));
#19678=CARTESIAN_POINT('Ctrl Pts',(1.03923048454133,0.846691919836082,1.8));
#19679=CARTESIAN_POINT('Ctrl Pts',(0.,0.905025253169415,1.8));
#19680=CARTESIAN_POINT('Ctrl Pts',(-1.03923048454133,0.963358586502749,
1.8));
#19681=CARTESIAN_POINT('Ctrl Pts',(-1.55884572681199,1.02169191983608,0.9));
#19682=CARTESIAN_POINT('Ctrl Pts',(-2.07846096908265,1.08002525316942,1.27269028646989E-16));
#19683=CARTESIAN_POINT('Ctrl Pts',(-1.55884572681199,1.13835858650275,-0.9));
#19684=CARTESIAN_POINT('Ctrl Pts',(-1.03923048454133,1.19669191983608,-1.8));
#19685=CARTESIAN_POINT('Ctrl Pts',(-2.20436423846524E-16,1.25502525316941,
-1.8));
#19686=CARTESIAN_POINT('Ctrl Pts',(1.03923048454133,1.31335858650275,-1.8));
#19687=CARTESIAN_POINT('Ctrl Pts',(1.55884572681199,1.37169191983608,-0.900000000000001));
#19688=CARTESIAN_POINT('Ctrl Pts',(2.07846096908265,1.43002525316941,-3.81807085940967E-16));
#19689=CARTESIAN_POINT('Ctrl Pts',(1.55884572681199,1.48835858650275,0.899999999999999));
#19690=CARTESIAN_POINT('Ctrl Pts',(1.03923048454133,1.54669191983608,1.8));
#19691=CARTESIAN_POINT('Ctrl Pts',(0.,1.60502525316941,1.8));
#19692=CARTESIAN_POINT('Ctrl Pts',(-1.03923048454133,1.66335858650275,1.8));
#19693=CARTESIAN_POINT('Ctrl Pts',(-1.55884572681199,1.72169191983608,0.9));
#19694=CARTESIAN_POINT('Ctrl Pts',(-2.07846096908265,1.78002525316941,1.27269028646989E-16));
#19695=CARTESIAN_POINT('Ctrl Pts',(-1.55884572681199,1.83835858650275,-0.9));
#19696=CARTESIAN_POINT('Ctrl Pts',(-1.03923048454133,1.89669191983608,-1.8));
#19697=CARTESIAN_POINT('Ctrl Pts',(-2.20436423846524E-16,1.95502525316941,
-1.8));
#19698=CARTESIAN_POINT('Ctrl Pts',(1.03923048454133,2.01335858650275,-1.8));
#19699=CARTESIAN_POINT('Ctrl Pts',(1.55884572681199,2.07169191983608,-0.900000000000001));
#19700=CARTESIAN_POINT('Ctrl Pts',(2.07846096908265,2.13002525316941,-3.81807085940967E-16));
#19701=CARTESIAN_POINT('Ctrl Pts',(1.55884572681199,2.18835858650275,0.899999999999999));
#19702=CARTESIAN_POINT('Ctrl Pts',(1.03923048454133,2.24669191983608,1.8));
#19703=CARTESIAN_POINT('Ctrl Pts',(0.,2.30502525316941,1.8));
#19704=CARTESIAN_POINT('Ctrl Pts',(-1.03923048454133,2.36335858650275,1.8));
#19705=CARTESIAN_POINT('Ctrl Pts',(-1.55884572681199,2.42169191983608,0.9));
#19706=CARTESIAN_POINT('Ctrl Pts',(-2.07846096908265,2.48002525316941,1.27269028646989E-16));
#19707=CARTESIAN_POINT('Ctrl Pts',(-1.55884572681199,2.53835858650275,-0.9));
#19708=CARTESIAN_POINT('Ctrl Pts',(-1.03923048454133,2.59669191983608,-1.8));
#19709=CARTESIAN_POINT('Ctrl Pts',(-2.20436423846524E-16,2.65502525316941,
-1.8));
#19710=CARTESIAN_POINT('Ctrl Pts',(1.03923048454133,2.71335858650274,-1.8));
#19711=CARTESIAN_POINT('Ctrl Pts',(1.55884572681199,2.77169191983608,-0.900000000000001));
#19712=CARTESIAN_POINT('Ctrl Pts',(2.07846096908265,2.83002525316941,-3.81807085940967E-16));
#19713=CARTESIAN_POINT('Ctrl Pts',(1.55884572681199,2.88835858650274,0.899999999999999));
#19714=CARTESIAN_POINT('Ctrl Pts',(1.03923048454133,2.94669191983608,1.8));
#19715=CARTESIAN_POINT('Ctrl Pts',(0.,3.00502525316941,1.8));
#19716=CARTESIAN_POINT('Ctrl Pts',(-1.03923048454133,3.06335858650274,1.8));
#19717=CARTESIAN_POINT('Ctrl Pts',(-1.55884572681199,3.12169191983608,0.9));
#19718=CARTESIAN_POINT('Ctrl Pts',(-2.07846096908265,3.18002525316941,1.27269028646989E-16));
#19719=CARTESIAN_POINT('Ctrl Pts',(-1.55884572681199,3.23835858650274,-0.9));
#19720=CARTESIAN_POINT('Ctrl Pts',(-1.03923048454133,3.29669191983608,-1.8));
#19721=CARTESIAN_POINT('Ctrl Pts',(-2.20436423846524E-16,3.35502525316941,
-1.8));
#19722=CARTESIAN_POINT('Ctrl Pts',(1.03923048454133,3.41335858650274,-1.8));
#19723=CARTESIAN_POINT('Ctrl Pts',(1.55884572681199,3.47169191983608,-0.900000000000001));
#19724=CARTESIAN_POINT('Ctrl Pts',(2.07846096908265,3.53002525316941,-3.81807085940967E-16));
#19725=CARTESIAN_POINT('Ctrl Pts',(1.55884572681199,3.58835858650274,0.899999999999999));
#19726=CARTESIAN_POINT('Ctrl Pts',(1.03923048454133,3.64669191983608,1.8));
#19727=CARTESIAN_POINT('Ctrl Pts',(0.,3.70502525316941,1.8));
#19728=CARTESIAN_POINT('Ctrl Pts',(-1.03923048454133,3.76335858650274,1.8));
#19729=CARTESIAN_POINT('Ctrl Pts',(-1.55884572681199,3.82169191983608,0.9));
#19730=CARTESIAN_POINT('Ctrl Pts',(-2.07846096908265,3.88002525316941,1.27269028646989E-16));
#19731=CARTESIAN_POINT('Ctrl Pts',(-1.55884572681199,3.93835858650274,-0.9));
#19732=CARTESIAN_POINT('Ctrl Pts',(-1.03923048454133,3.99669191983608,-1.8));
#19733=CARTESIAN_POINT('Ctrl Pts',(-2.20436423846524E-16,4.05502525316941,
-1.8));
#19734=CARTESIAN_POINT('Ctrl Pts',(1.03923048454133,4.11335858650274,-1.8));
#19735=CARTESIAN_POINT('Ctrl Pts',(1.55884572681199,4.17169191983608,-0.900000000000001));
#19736=CARTESIAN_POINT('Ctrl Pts',(2.07846096908265,4.23002525316941,-3.81807085940967E-16));
#19737=CARTESIAN_POINT('Ctrl Pts',(1.55884572681199,4.28835858650274,0.899999999999999));
#19738=CARTESIAN_POINT('Ctrl Pts',(1.03923048454133,4.34669191983608,1.8));
#19739=CARTESIAN_POINT('Ctrl Pts',(0.,4.40502525316941,1.8));
#19740=CARTESIAN_POINT('Ctrl Pts',(0.,0.35,1.94497474683058));
#19741=CARTESIAN_POINT('Ctrl Pts',(-1.12293169364966,0.408333333333333,
1.94497474683058));
#19742=CARTESIAN_POINT('Ctrl Pts',(-1.68439754047449,0.466666666666666,
0.972487373415292));
#19743=CARTESIAN_POINT('Ctrl Pts',(-2.24586338729932,0.525,1.37519470428917E-16));
#19744=CARTESIAN_POINT('Ctrl Pts',(-1.68439754047449,0.583333333333333,
-0.972487373415291));
#19745=CARTESIAN_POINT('Ctrl Pts',(-1.12293169364966,0.641666666666666,
-1.94497474683058));
#19746=CARTESIAN_POINT('Ctrl Pts',(-2.38190709812851E-16,0.699999999999999,
-1.94497474683058));
#19747=CARTESIAN_POINT('Ctrl Pts',(1.12293169364966,0.758333333333333,-1.94497474683058));
#19748=CARTESIAN_POINT('Ctrl Pts',(1.68439754047449,0.816666666666666,-0.972487373415292));
#19749=CARTESIAN_POINT('Ctrl Pts',(2.24586338729932,0.874999999999999,-4.12558411286752E-16));
#19750=CARTESIAN_POINT('Ctrl Pts',(1.68439754047449,0.933333333333332,0.97248737341529));
#19751=CARTESIAN_POINT('Ctrl Pts',(1.12293169364966,0.991666666666665,1.94497474683058));
#19752=CARTESIAN_POINT('Ctrl Pts',(0.,1.05,1.94497474683058));
#19753=CARTESIAN_POINT('Ctrl Pts',(-1.12293169364966,1.10833333333333,1.94497474683058));
#19754=CARTESIAN_POINT('Ctrl Pts',(-1.68439754047449,1.16666666666666,0.972487373415292));
#19755=CARTESIAN_POINT('Ctrl Pts',(-2.24586338729932,1.225,1.37519470428917E-16));
#19756=CARTESIAN_POINT('Ctrl Pts',(-1.68439754047449,1.28333333333333,-0.972487373415291));
#19757=CARTESIAN_POINT('Ctrl Pts',(-1.12293169364966,1.34166666666667,-1.94497474683058));
#19758=CARTESIAN_POINT('Ctrl Pts',(-2.38190709812851E-16,1.4,-1.94497474683058));
#19759=CARTESIAN_POINT('Ctrl Pts',(1.12293169364966,1.45833333333333,-1.94497474683058));
#19760=CARTESIAN_POINT('Ctrl Pts',(1.68439754047449,1.51666666666666,-0.972487373415292));
#19761=CARTESIAN_POINT('Ctrl Pts',(2.24586338729932,1.575,-4.12558411286752E-16));
#19762=CARTESIAN_POINT('Ctrl Pts',(1.68439754047449,1.63333333333333,0.97248737341529));
#19763=CARTESIAN_POINT('Ctrl Pts',(1.12293169364966,1.69166666666666,1.94497474683058));
#19764=CARTESIAN_POINT('Ctrl Pts',(0.,1.75,1.94497474683058));
#19765=CARTESIAN_POINT('Ctrl Pts',(-1.12293169364966,1.80833333333333,1.94497474683058));
#19766=CARTESIAN_POINT('Ctrl Pts',(-1.68439754047449,1.86666666666666,0.972487373415292));
#19767=CARTESIAN_POINT('Ctrl Pts',(-2.24586338729932,1.925,1.37519470428917E-16));
#19768=CARTESIAN_POINT('Ctrl Pts',(-1.68439754047449,1.98333333333333,-0.972487373415291));
#19769=CARTESIAN_POINT('Ctrl Pts',(-1.12293169364966,2.04166666666666,-1.94497474683058));
#19770=CARTESIAN_POINT('Ctrl Pts',(-2.38190709812851E-16,2.1,-1.94497474683058));
#19771=CARTESIAN_POINT('Ctrl Pts',(1.12293169364966,2.15833333333333,-1.94497474683058));
#19772=CARTESIAN_POINT('Ctrl Pts',(1.68439754047449,2.21666666666666,-0.972487373415292));
#19773=CARTESIAN_POINT('Ctrl Pts',(2.24586338729932,2.275,-4.12558411286752E-16));
#19774=CARTESIAN_POINT('Ctrl Pts',(1.68439754047449,2.33333333333333,0.97248737341529));
#19775=CARTESIAN_POINT('Ctrl Pts',(1.12293169364966,2.39166666666666,1.94497474683058));
#19776=CARTESIAN_POINT('Ctrl Pts',(0.,2.45,1.94497474683058));
#19777=CARTESIAN_POINT('Ctrl Pts',(-1.12293169364966,2.50833333333333,1.94497474683058));
#19778=CARTESIAN_POINT('Ctrl Pts',(-1.68439754047449,2.56666666666666,0.972487373415292));
#19779=CARTESIAN_POINT('Ctrl Pts',(-2.24586338729932,2.62499999999999,1.37519470428917E-16));
#19780=CARTESIAN_POINT('Ctrl Pts',(-1.68439754047449,2.68333333333333,-0.972487373415291));
#19781=CARTESIAN_POINT('Ctrl Pts',(-1.12293169364966,2.74166666666666,-1.94497474683058));
#19782=CARTESIAN_POINT('Ctrl Pts',(-2.38190709812851E-16,2.8,-1.94497474683058));
#19783=CARTESIAN_POINT('Ctrl Pts',(1.12293169364966,2.85833333333333,-1.94497474683058));
#19784=CARTESIAN_POINT('Ctrl Pts',(1.68439754047449,2.91666666666666,-0.972487373415292));
#19785=CARTESIAN_POINT('Ctrl Pts',(2.24586338729932,2.97499999999999,-4.12558411286752E-16));
#19786=CARTESIAN_POINT('Ctrl Pts',(1.68439754047449,3.03333333333333,0.97248737341529));
#19787=CARTESIAN_POINT('Ctrl Pts',(1.12293169364966,3.09166666666666,1.94497474683058));
#19788=CARTESIAN_POINT('Ctrl Pts',(0.,3.14999999999999,1.94497474683058));
#19789=CARTESIAN_POINT('Ctrl Pts',(-1.12293169364966,3.20833333333333,1.94497474683058));
#19790=CARTESIAN_POINT('Ctrl Pts',(-1.68439754047449,3.26666666666666,0.972487373415292));
#19791=CARTESIAN_POINT('Ctrl Pts',(-2.24586338729932,3.32499999999999,1.37519470428917E-16));
#19792=CARTESIAN_POINT('Ctrl Pts',(-1.68439754047449,3.38333333333333,-0.972487373415291));
#19793=CARTESIAN_POINT('Ctrl Pts',(-1.12293169364966,3.44166666666666,-1.94497474683058));
#19794=CARTESIAN_POINT('Ctrl Pts',(-2.38190709812851E-16,3.49999999999999,
-1.94497474683058));
#19795=CARTESIAN_POINT('Ctrl Pts',(1.12293169364966,3.55833333333333,-1.94497474683058));
#19796=CARTESIAN_POINT('Ctrl Pts',(1.68439754047449,3.61666666666666,-0.972487373415292));
#19797=CARTESIAN_POINT('Ctrl Pts',(2.24586338729932,3.67499999999999,-4.12558411286752E-16));
#19798=CARTESIAN_POINT('Ctrl Pts',(1.68439754047449,3.73333333333333,0.97248737341529));
#19799=CARTESIAN_POINT('Ctrl Pts',(1.12293169364966,3.79166666666666,1.94497474683058));
#19800=CARTESIAN_POINT('Ctrl Pts',(0.,3.84999999999999,1.94497474683058));
#19801=CARTESIAN_POINT('Ctrl Pts',(-1.12293169364966,3.90833333333333,1.94497474683058));
#19802=CARTESIAN_POINT('Ctrl Pts',(-1.68439754047449,3.96666666666666,0.972487373415292));
#19803=CARTESIAN_POINT('Ctrl Pts',(-2.24586338729932,4.02499999999999,1.37519470428917E-16));
#19804=CARTESIAN_POINT('Ctrl Pts',(-1.68439754047449,4.08333333333333,-0.972487373415291));
#19805=CARTESIAN_POINT('Ctrl Pts',(-1.12293169364966,4.14166666666666,-1.94497474683058));
#19806=CARTESIAN_POINT('Ctrl Pts',(-2.38190709812851E-16,4.19999999999999,
-1.94497474683058));
#19807=CARTESIAN_POINT('Ctrl Pts',(1.12293169364966,4.25833333333332,-1.94497474683058));
#19808=CARTESIAN_POINT('Ctrl Pts',(1.68439754047449,4.31666666666666,-0.972487373415292));
#19809=CARTESIAN_POINT('Ctrl Pts',(2.24586338729932,4.37499999999999,-4.12558411286752E-16));
#19810=CARTESIAN_POINT('Ctrl Pts',(1.68439754047449,4.43333333333332,0.97248737341529));
#19811=CARTESIAN_POINT('Ctrl Pts',(1.12293169364966,4.49166666666666,1.94497474683058));
#19812=CARTESIAN_POINT('Ctrl Pts',(0.,4.54999999999999,1.94497474683058));
#19813=CARTESIAN_POINT('Ctrl Pts',(0.,0.35,2.15));
#19814=CARTESIAN_POINT('Ctrl Pts',(-1.2413030787577,0.408333333333333,2.15));
#19815=CARTESIAN_POINT('Ctrl Pts',(-1.86195461813654,0.466666666666667,
1.075));
#19816=CARTESIAN_POINT('Ctrl Pts',(-2.48260615751539,0.525,1.52015784217237E-16));
#19817=CARTESIAN_POINT('Ctrl Pts',(-1.86195461813654,0.583333333333333,
-1.075));
#19818=CARTESIAN_POINT('Ctrl Pts',(-1.2413030787577,0.641666666666666,-2.15));
#19819=CARTESIAN_POINT('Ctrl Pts',(-2.63299061816681E-16,0.699999999999999,
-2.15));
#19820=CARTESIAN_POINT('Ctrl Pts',(1.24130307875769,0.758333333333333,-2.15));
#19821=CARTESIAN_POINT('Ctrl Pts',(1.86195461813654,0.816666666666666,-1.075));
#19822=CARTESIAN_POINT('Ctrl Pts',(2.48260615751539,0.874999999999999,-4.5604735265171E-16));
#19823=CARTESIAN_POINT('Ctrl Pts',(1.86195461813654,0.933333333333332,1.075));
#19824=CARTESIAN_POINT('Ctrl Pts',(1.2413030787577,0.991666666666666,2.15));
#19825=CARTESIAN_POINT('Ctrl Pts',(0.,1.05,2.15));
#19826=CARTESIAN_POINT('Ctrl Pts',(-1.2413030787577,1.10833333333333,2.15));
#19827=CARTESIAN_POINT('Ctrl Pts',(-1.86195461813654,1.16666666666667,1.075));
#19828=CARTESIAN_POINT('Ctrl Pts',(-2.48260615751539,1.225,1.52015784217237E-16));
#19829=CARTESIAN_POINT('Ctrl Pts',(-1.86195461813654,1.28333333333333,-1.075));
#19830=CARTESIAN_POINT('Ctrl Pts',(-1.2413030787577,1.34166666666666,-2.15));
#19831=CARTESIAN_POINT('Ctrl Pts',(-2.63299061816681E-16,1.4,-2.15));
#19832=CARTESIAN_POINT('Ctrl Pts',(1.24130307875769,1.45833333333333,-2.15));
#19833=CARTESIAN_POINT('Ctrl Pts',(1.86195461813654,1.51666666666666,-1.075));
#19834=CARTESIAN_POINT('Ctrl Pts',(2.48260615751539,1.575,-4.5604735265171E-16));
#19835=CARTESIAN_POINT('Ctrl Pts',(1.86195461813654,1.63333333333333,1.075));
#19836=CARTESIAN_POINT('Ctrl Pts',(1.2413030787577,1.69166666666666,2.15));
#19837=CARTESIAN_POINT('Ctrl Pts',(0.,1.75,2.15));
#19838=CARTESIAN_POINT('Ctrl Pts',(-1.2413030787577,1.80833333333333,2.15));
#19839=CARTESIAN_POINT('Ctrl Pts',(-1.86195461813654,1.86666666666666,1.075));
#19840=CARTESIAN_POINT('Ctrl Pts',(-2.48260615751539,1.925,1.52015784217237E-16));
#19841=CARTESIAN_POINT('Ctrl Pts',(-1.86195461813654,1.98333333333333,-1.075));
#19842=CARTESIAN_POINT('Ctrl Pts',(-1.2413030787577,2.04166666666666,-2.15));
#19843=CARTESIAN_POINT('Ctrl Pts',(-2.63299061816681E-16,2.1,-2.15));
#19844=CARTESIAN_POINT('Ctrl Pts',(1.24130307875769,2.15833333333333,-2.15));
#19845=CARTESIAN_POINT('Ctrl Pts',(1.86195461813654,2.21666666666666,-1.075));
#19846=CARTESIAN_POINT('Ctrl Pts',(2.48260615751539,2.275,-4.5604735265171E-16));
#19847=CARTESIAN_POINT('Ctrl Pts',(1.86195461813654,2.33333333333333,1.075));
#19848=CARTESIAN_POINT('Ctrl Pts',(1.2413030787577,2.39166666666666,2.15));
#19849=CARTESIAN_POINT('Ctrl Pts',(0.,2.45,2.15));
#19850=CARTESIAN_POINT('Ctrl Pts',(-1.2413030787577,2.50833333333333,2.15));
#19851=CARTESIAN_POINT('Ctrl Pts',(-1.86195461813654,2.56666666666666,1.075));
#19852=CARTESIAN_POINT('Ctrl Pts',(-2.48260615751539,2.625,1.52015784217237E-16));
#19853=CARTESIAN_POINT('Ctrl Pts',(-1.86195461813654,2.68333333333333,-1.075));
#19854=CARTESIAN_POINT('Ctrl Pts',(-1.2413030787577,2.74166666666666,-2.15));
#19855=CARTESIAN_POINT('Ctrl Pts',(-2.63299061816681E-16,2.8,-2.15));
#19856=CARTESIAN_POINT('Ctrl Pts',(1.24130307875769,2.85833333333333,-2.15));
#19857=CARTESIAN_POINT('Ctrl Pts',(1.86195461813654,2.91666666666666,-1.075));
#19858=CARTESIAN_POINT('Ctrl Pts',(2.48260615751539,2.97499999999999,-4.5604735265171E-16));
#19859=CARTESIAN_POINT('Ctrl Pts',(1.86195461813654,3.03333333333333,1.075));
#19860=CARTESIAN_POINT('Ctrl Pts',(1.2413030787577,3.09166666666666,2.15));
#19861=CARTESIAN_POINT('Ctrl Pts',(0.,3.15,2.15));
#19862=CARTESIAN_POINT('Ctrl Pts',(-1.2413030787577,3.20833333333333,2.15));
#19863=CARTESIAN_POINT('Ctrl Pts',(-1.86195461813654,3.26666666666666,1.075));
#19864=CARTESIAN_POINT('Ctrl Pts',(-2.48260615751539,3.32499999999999,1.52015784217237E-16));
#19865=CARTESIAN_POINT('Ctrl Pts',(-1.86195461813654,3.38333333333333,-1.075));
#19866=CARTESIAN_POINT('Ctrl Pts',(-1.2413030787577,3.44166666666666,-2.15));
#19867=CARTESIAN_POINT('Ctrl Pts',(-2.63299061816681E-16,3.49999999999999,
-2.15));
#19868=CARTESIAN_POINT('Ctrl Pts',(1.24130307875769,3.55833333333333,-2.15));
#19869=CARTESIAN_POINT('Ctrl Pts',(1.86195461813654,3.61666666666666,-1.075));
#19870=CARTESIAN_POINT('Ctrl Pts',(2.48260615751539,3.67499999999999,-4.5604735265171E-16));
#19871=CARTESIAN_POINT('Ctrl Pts',(1.86195461813654,3.73333333333333,1.075));
#19872=CARTESIAN_POINT('Ctrl Pts',(1.2413030787577,3.79166666666666,2.15));
#19873=CARTESIAN_POINT('Ctrl Pts',(0.,3.84999999999999,2.15));
#19874=CARTESIAN_POINT('Ctrl Pts',(-1.2413030787577,3.90833333333333,2.15));
#19875=CARTESIAN_POINT('Ctrl Pts',(-1.86195461813654,3.96666666666666,1.075));
#19876=CARTESIAN_POINT('Ctrl Pts',(-2.48260615751539,4.02499999999999,1.52015784217237E-16));
#19877=CARTESIAN_POINT('Ctrl Pts',(-1.86195461813654,4.08333333333333,-1.075));
#19878=CARTESIAN_POINT('Ctrl Pts',(-1.2413030787577,4.14166666666666,-2.15));
#19879=CARTESIAN_POINT('Ctrl Pts',(-2.63299061816681E-16,4.19999999999999,
-2.15));
#19880=CARTESIAN_POINT('Ctrl Pts',(1.24130307875769,4.25833333333333,-2.15));
#19881=CARTESIAN_POINT('Ctrl Pts',(1.86195461813654,4.31666666666666,-1.075));
#19882=CARTESIAN_POINT('Ctrl Pts',(2.48260615751539,4.37499999999999,-4.5604735265171E-16));
#19883=CARTESIAN_POINT('Ctrl Pts',(1.86195461813654,4.43333333333333,1.075));
#19884=CARTESIAN_POINT('Ctrl Pts',(1.2413030787577,4.49166666666666,2.15));
#19885=CARTESIAN_POINT('Ctrl Pts',(0.,4.54999999999999,2.15));
#19886=CARTESIAN_POINT('',(-7.40933783759325E-14,4.2,1.8));
#19887=CARTESIAN_POINT('',(-8.82371251094361E-14,4.55,2.15));
#19888=CARTESIAN_POINT('Origin',(-1.80160437084306E-13,4.2,2.15));
#19889=CARTESIAN_POINT('',(-8.87637232330694E-14,3.85,2.15));
#19890=CARTESIAN_POINT('Ctrl Pts',(1.05346240894046E-14,3.84999999999999,
2.15));
#19891=CARTESIAN_POINT('Ctrl Pts',(-1.24130307875769,3.90833333333333,2.15));
#19892=CARTESIAN_POINT('Ctrl Pts',(-1.86195461813654,3.96666666666666,1.075));
#19893=CARTESIAN_POINT('Ctrl Pts',(-2.48260615751539,4.02499999999999,1.67263463193154E-14));
#19894=CARTESIAN_POINT('Ctrl Pts',(-1.86195461813655,4.08333333333333,-1.07499999999999));
#19895=CARTESIAN_POINT('Ctrl Pts',(-1.2413030787577,4.14166666666666,-2.15));
#19896=CARTESIAN_POINT('Ctrl Pts',(-1.07979231512212E-14,4.19999999999999,
-2.15));
#19897=CARTESIAN_POINT('Ctrl Pts',(1.24130307875769,4.25833333333332,-2.15));
#19898=CARTESIAN_POINT('Ctrl Pts',(1.86195461813654,4.31666666666666,-1.07500000000001));
#19899=CARTESIAN_POINT('Ctrl Pts',(2.48260615751539,4.37499999999999,-8.21038903287055E-15));
#19900=CARTESIAN_POINT('Ctrl Pts',(1.86195461813655,4.43333333333332,1.07499999999999));
#19901=CARTESIAN_POINT('Ctrl Pts',(1.24130307875771,4.49166666666666,2.14999999999999));
#19902=CARTESIAN_POINT('Ctrl Pts',(-8.82371251094361E-14,4.55,2.15));
#19903=CARTESIAN_POINT('',(2.63299061816681E-16,0.349999999999999,2.15));
#19904=CARTESIAN_POINT('Ctrl Pts',(2.63299061816681E-16,0.349999999999999,
2.15));
#19905=CARTESIAN_POINT('Ctrl Pts',(-1.24130307875769,0.408333333333333,
2.15));
#19906=CARTESIAN_POINT('Ctrl Pts',(-1.86195461813654,0.466666666666666,
1.075));
#19907=CARTESIAN_POINT('Ctrl Pts',(-2.48260615751539,0.524999999999999,
4.5604735265171E-16));
#19908=CARTESIAN_POINT('Ctrl Pts',(-1.86195461813654,0.583333333333332,
-1.075));
#19909=CARTESIAN_POINT('Ctrl Pts',(-1.2413030787577,0.641666666666665,-2.15));
#19910=CARTESIAN_POINT('Ctrl Pts',(-5.26598123633362E-16,0.699999999999999,
-2.15));
#19911=CARTESIAN_POINT('Ctrl Pts',(1.24130307875769,0.758333333333332,-2.15));
#19912=CARTESIAN_POINT('Ctrl Pts',(1.86195461813654,0.816666666666665,-1.075));
#19913=CARTESIAN_POINT('Ctrl Pts',(2.48260615751539,0.874999999999999,-7.60078921086183E-16));
#19914=CARTESIAN_POINT('Ctrl Pts',(1.86195461813654,0.933333333333332,1.075));
#19915=CARTESIAN_POINT('Ctrl Pts',(1.2413030787577,0.991666666666665,2.15));
#19916=CARTESIAN_POINT('Ctrl Pts',(7.89897185450043E-16,1.05,2.15));
#19917=CARTESIAN_POINT('Ctrl Pts',(-1.24130307875769,1.10833333333333,2.15));
#19918=CARTESIAN_POINT('Ctrl Pts',(-1.86195461813654,1.16666666666666,1.075));
#19919=CARTESIAN_POINT('Ctrl Pts',(-2.48260615751539,1.225,3.26910770324048E-15));
#19920=CARTESIAN_POINT('Ctrl Pts',(-1.86195461813654,1.28333333333333,-1.075));
#19921=CARTESIAN_POINT('Ctrl Pts',(-1.2413030787577,1.34166666666666,-2.15));
#19922=CARTESIAN_POINT('Ctrl Pts',(-1.05319624726672E-15,1.4,-2.15));
#19923=CARTESIAN_POINT('Ctrl Pts',(1.24130307875769,1.45833333333333,-2.15));
#19924=CARTESIAN_POINT('Ctrl Pts',(1.86195461813654,1.51666666666666,-1.075));
#19925=CARTESIAN_POINT('Ctrl Pts',(2.48260615751539,1.575,-1.36814205795513E-15));
#19926=CARTESIAN_POINT('Ctrl Pts',(1.86195461813654,1.63333333333333,1.075));
#19927=CARTESIAN_POINT('Ctrl Pts',(1.2413030787577,1.69166666666666,2.15));
#19928=CARTESIAN_POINT('Ctrl Pts',(1.3164953090834E-15,1.75,2.15));
#19929=CARTESIAN_POINT('Ctrl Pts',(-1.24130307875769,1.80833333333333,2.15));
#19930=CARTESIAN_POINT('Ctrl Pts',(-1.86195461813654,1.86666666666666,1.075));
#19931=CARTESIAN_POINT('Ctrl Pts',(-2.48260615751539,1.925,6.08216805382924E-15));
#19932=CARTESIAN_POINT('Ctrl Pts',(-1.86195461813654,1.98333333333333,-1.075));
#19933=CARTESIAN_POINT('Ctrl Pts',(-1.2413030787577,2.04166666666666,-2.15));
#19934=CARTESIAN_POINT('Ctrl Pts',(-5.39896157561062E-15,2.1,-2.15));
#19935=CARTESIAN_POINT('Ctrl Pts',(1.24130307875769,2.15833333333333,-2.15));
#19936=CARTESIAN_POINT('Ctrl Pts',(1.86195461813654,2.21666666666666,-1.075));
#19937=CARTESIAN_POINT('Ctrl Pts',(2.48260615751539,2.275,-6.38619962226372E-15));
#19938=CARTESIAN_POINT('Ctrl Pts',(1.86195461813655,2.33333333333333,1.07499999999999));
#19939=CARTESIAN_POINT('Ctrl Pts',(1.2413030787577,2.39166666666666,2.15));
#19940=CARTESIAN_POINT('Ctrl Pts',(1.84309343271677E-15,2.45,2.15));
#19941=CARTESIAN_POINT('Ctrl Pts',(-1.24130307875769,2.50833333333333,2.15));
#19942=CARTESIAN_POINT('Ctrl Pts',(-1.86195461813654,2.56666666666666,1.075));
#19943=CARTESIAN_POINT('Ctrl Pts',(-2.48260615751539,2.62499999999999,6.69023119069819E-15));
#19944=CARTESIAN_POINT('Ctrl Pts',(-1.86195461813655,2.68333333333333,-1.07499999999999));
#19945=CARTESIAN_POINT('Ctrl Pts',(-1.2413030787577,2.74166666666666,-2.14999999999999));
#19946=CARTESIAN_POINT('Ctrl Pts',(-2.10639249453345E-15,2.79999999999999,
-2.15));
#19947=CARTESIAN_POINT('Ctrl Pts',(1.24130307875769,2.85833333333333,-2.15));
#19948=CARTESIAN_POINT('Ctrl Pts',(1.86195461813654,2.91666666666666,-1.075));
#19949=CARTESIAN_POINT('Ctrl Pts',(2.48260615751539,2.97499999999999,-6.99426275913266E-15));
#19950=CARTESIAN_POINT('Ctrl Pts',(1.86195461813655,3.03333333333333,1.07499999999999));
#19951=CARTESIAN_POINT('Ctrl Pts',(1.2413030787577,3.09166666666666,2.14999999999999));
#19952=CARTESIAN_POINT('Ctrl Pts',(2.36969155635013E-15,3.14999999999999,
2.15));
#19953=CARTESIAN_POINT('Ctrl Pts',(-1.24130307875769,3.20833333333333,2.15));
#19954=CARTESIAN_POINT('Ctrl Pts',(-1.86195461813654,3.26666666666666,1.075));
#19955=CARTESIAN_POINT('Ctrl Pts',(-2.48260615751539,3.32499999999999,7.29829432756713E-15));
#19956=CARTESIAN_POINT('Ctrl Pts',(-1.86195461813655,3.38333333333333,-1.07499999999999));
#19957=CARTESIAN_POINT('Ctrl Pts',(-1.2413030787577,3.44166666666666,-2.14999999999999));
#19958=CARTESIAN_POINT('Ctrl Pts',(-1.02713250275879E-14,3.49999999999999,
-2.15));
#19959=CARTESIAN_POINT('Ctrl Pts',(1.24130307875769,3.55833333333333,-2.15));
#19960=CARTESIAN_POINT('Ctrl Pts',(1.86195461813654,3.61666666666666,-1.075));
#19961=CARTESIAN_POINT('Ctrl Pts',(2.48260615751539,3.67499999999999,-7.60232589600161E-15));
#19962=CARTESIAN_POINT('Ctrl Pts',(1.86195461813655,3.73333333333333,1.07499999999999));
#19963=CARTESIAN_POINT('Ctrl Pts',(1.2413030787577,3.79166666666666,2.14999999999999));
#19964=CARTESIAN_POINT('Ctrl Pts',(1.05346240894046E-14,3.84999999999999,
2.15));
#19965=CARTESIAN_POINT('',(0.,0.,1.8));
#19966=CARTESIAN_POINT('Origin',(0.,0.,2.15));
#19967=CARTESIAN_POINT('Ctrl Pts',(0.,0.,1.8));
#19968=CARTESIAN_POINT('Ctrl Pts',(-1.03923048454133,0.0583333333333332,
1.8));
#19969=CARTESIAN_POINT('Ctrl Pts',(-1.55884572681199,0.116666666666666,
0.9));
#19970=CARTESIAN_POINT('Ctrl Pts',(-2.07846096908265,0.175,1.27269028646989E-16));
#19971=CARTESIAN_POINT('Ctrl Pts',(-1.55884572681199,0.233333333333333,
-0.9));
#19972=CARTESIAN_POINT('Ctrl Pts',(-1.03923048454133,0.291666666666666,
-1.8));
#19973=CARTESIAN_POINT('Ctrl Pts',(-2.20436423846524E-16,0.349999999999999,
-1.8));
#19974=CARTESIAN_POINT('Ctrl Pts',(1.03923048454133,0.408333333333333,-1.8));
#19975=CARTESIAN_POINT('Ctrl Pts',(1.55884572681199,0.466666666666666,-0.900000000000001));
#19976=CARTESIAN_POINT('Ctrl Pts',(2.07846096908265,0.524999999999999,-3.81807085940967E-16));
#19977=CARTESIAN_POINT('Ctrl Pts',(1.55884572681199,0.583333333333332,0.899999999999999));
#19978=CARTESIAN_POINT('Ctrl Pts',(1.03923048454133,0.641666666666665,1.8));
#19979=CARTESIAN_POINT('Ctrl Pts',(4.40872847693047E-16,0.699999999999999,
1.8));
#19980=CARTESIAN_POINT('Ctrl Pts',(-1.03923048454132,0.758333333333332,
1.8));
#19981=CARTESIAN_POINT('Ctrl Pts',(-1.55884572681199,0.816666666666665,
0.900000000000001));
#19982=CARTESIAN_POINT('Ctrl Pts',(-2.07846096908265,0.874999999999998,
2.48238932216317E-15));
#19983=CARTESIAN_POINT('Ctrl Pts',(-1.55884572681199,0.933333333333332,
-0.899999999999999));
#19984=CARTESIAN_POINT('Ctrl Pts',(-1.03923048454133,0.991666666666665,
-1.8));
#19985=CARTESIAN_POINT('Ctrl Pts',(-6.61309271539571E-16,1.05,-1.8));
#19986=CARTESIAN_POINT('Ctrl Pts',(1.03923048454132,1.10833333333333,-1.8));
#19987=CARTESIAN_POINT('Ctrl Pts',(1.55884572681199,1.16666666666666,-0.900000000000002));
#19988=CARTESIAN_POINT('Ctrl Pts',(2.07846096908265,1.225,-8.90883200528922E-16));
#19989=CARTESIAN_POINT('Ctrl Pts',(1.55884572681199,1.28333333333333,0.899999999999998));
#19990=CARTESIAN_POINT('Ctrl Pts',(1.03923048454133,1.34166666666666,1.8));
#19991=CARTESIAN_POINT('Ctrl Pts',(8.81745695386094E-16,1.4,1.8));
#19992=CARTESIAN_POINT('Ctrl Pts',(-1.03923048454132,1.45833333333333,1.8));
#19993=CARTESIAN_POINT('Ctrl Pts',(-1.55884572681199,1.51666666666666,0.900000000000003));
#19994=CARTESIAN_POINT('Ctrl Pts',(-2.07846096908265,1.575,4.83750961567934E-15));
#19995=CARTESIAN_POINT('Ctrl Pts',(-1.55884572681199,1.63333333333333,-0.899999999999998));
#19996=CARTESIAN_POINT('Ctrl Pts',(-1.03923048454133,1.69166666666666,-1.8));
#19997=CARTESIAN_POINT('Ctrl Pts',(-4.29962443015307E-15,1.75,-1.8));
#19998=CARTESIAN_POINT('Ctrl Pts',(1.03923048454132,1.80833333333333,-1.8));
#19999=CARTESIAN_POINT('Ctrl Pts',(1.55884572681199,1.86666666666666,-0.900000000000003));
#20000=CARTESIAN_POINT('Ctrl Pts',(2.07846096908265,1.925,-5.09204767297332E-15));
#20001=CARTESIAN_POINT('Ctrl Pts',(1.55884572681199,1.98333333333333,0.899999999999995));
#20002=CARTESIAN_POINT('Ctrl Pts',(1.03923048454133,2.04166666666666,1.8));
#20003=CARTESIAN_POINT('Ctrl Pts',(1.32261854307914E-15,2.1,1.8));
#20004=CARTESIAN_POINT('Ctrl Pts',(-1.03923048454132,2.15833333333333,1.8));
#20005=CARTESIAN_POINT('Ctrl Pts',(-1.55884572681199,2.21666666666666,0.900000000000003));
#20006=CARTESIAN_POINT('Ctrl Pts',(-2.07846096908265,2.275,5.3465857302673E-15));
#20007=CARTESIAN_POINT('Ctrl Pts',(-1.55884572681199,2.33333333333333,-0.899999999999995));
#20008=CARTESIAN_POINT('Ctrl Pts',(-1.03923048454133,2.39166666666666,-1.8));
#20009=CARTESIAN_POINT('Ctrl Pts',(-1.54305496692567E-15,2.45,-1.8));
#20010=CARTESIAN_POINT('Ctrl Pts',(1.03923048454132,2.50833333333333,-1.8));
#20011=CARTESIAN_POINT('Ctrl Pts',(1.55884572681199,2.56666666666666,-0.900000000000003));
#20012=CARTESIAN_POINT('Ctrl Pts',(2.07846096908265,2.625,-5.60112378756128E-15));
#20013=CARTESIAN_POINT('Ctrl Pts',(1.55884572681199,2.68333333333333,0.899999999999995));
#20014=CARTESIAN_POINT('Ctrl Pts',(1.03923048454133,2.74166666666666,1.8));
#20015=CARTESIAN_POINT('Ctrl Pts',(1.76349139077219E-15,2.79999999999999,
1.8));
#20016=CARTESIAN_POINT('Ctrl Pts',(-1.03923048454132,2.85833333333333,1.8));
#20017=CARTESIAN_POINT('Ctrl Pts',(-1.55884572681199,2.91666666666666,0.900000000000003));
#20018=CARTESIAN_POINT('Ctrl Pts',(-2.07846096908265,2.97499999999999,5.85566184485525E-15));
#20019=CARTESIAN_POINT('Ctrl Pts',(-1.55884572681199,3.03333333333333,-0.899999999999995));
#20020=CARTESIAN_POINT('Ctrl Pts',(-1.03923048454133,3.09166666666666,-1.8));
#20021=CARTESIAN_POINT('Ctrl Pts',(-8.37881243645961E-15,3.14999999999999,
-1.8));
#20022=CARTESIAN_POINT('Ctrl Pts',(1.03923048454132,3.20833333333333,-1.8));
#20023=CARTESIAN_POINT('Ctrl Pts',(1.55884572681199,3.26666666666666,-0.900000000000004));
#20024=CARTESIAN_POINT('Ctrl Pts',(2.07846096908265,3.32499999999999,-6.11019990214923E-15));
#20025=CARTESIAN_POINT('Ctrl Pts',(1.55884572681199,3.38333333333333,0.899999999999995));
#20026=CARTESIAN_POINT('Ctrl Pts',(1.03923048454133,3.44166666666666,1.8));
#20027=CARTESIAN_POINT('Ctrl Pts',(8.59924886030614E-15,3.49999999999999,
1.8));
#20028=CARTESIAN_POINT('Ctrl Pts',(-1.03923048454132,3.55833333333333,1.8));
#20029=CARTESIAN_POINT('Ctrl Pts',(-1.55884572681199,3.61666666666666,0.900000000000004));
#20030=CARTESIAN_POINT('Ctrl Pts',(-2.07846096908265,3.67499999999999,1.37489146751561E-14));
#20031=CARTESIAN_POINT('Ctrl Pts',(-1.55884572681199,3.73333333333333,-0.899999999999994));
#20032=CARTESIAN_POINT('Ctrl Pts',(-1.03923048454133,3.79166666666666,-1.8));
#20033=CARTESIAN_POINT('Ctrl Pts',(-8.81968528415266E-15,3.84999999999999,
-1.8));
#20034=CARTESIAN_POINT('Ctrl Pts',(1.03923048454132,3.90833333333333,-1.8));
#20035=CARTESIAN_POINT('Ctrl Pts',(1.55884572681198,3.96666666666666,-0.90000000000001));
#20036=CARTESIAN_POINT('Ctrl Pts',(2.07846096908265,4.02499999999999,-6.61927601673719E-15));
#20037=CARTESIAN_POINT('Ctrl Pts',(1.558845726812,4.08333333333333,0.899999999999989));
#20038=CARTESIAN_POINT('Ctrl Pts',(1.03923048454133,4.14166666666666,1.8));
#20039=CARTESIAN_POINT('Ctrl Pts',(-7.40933783759325E-14,4.2,1.8));
#20040=CARTESIAN_POINT('Ctrl Pts',(0.,-0.35,2.15));
#20041=CARTESIAN_POINT('Ctrl Pts',(-1.2413030787577,-0.291666666666667,
2.15));
#20042=CARTESIAN_POINT('Ctrl Pts',(-1.86195461813654,-0.233333333333334,
1.075));
#20043=CARTESIAN_POINT('Ctrl Pts',(-2.48260615751539,-0.175,1.52015784217237E-16));
#20044=CARTESIAN_POINT('Ctrl Pts',(-1.86195461813654,-0.116666666666667,
-1.075));
#20045=CARTESIAN_POINT('Ctrl Pts',(-1.2413030787577,-0.058333333333334,
-2.15));
#20046=CARTESIAN_POINT('Ctrl Pts',(-2.63299061816681E-16,-7.58941520739853E-16,
-2.15));
#20047=CARTESIAN_POINT('Ctrl Pts',(1.24130307875769,0.0583333333333325,
-2.15));
#20048=CARTESIAN_POINT('Ctrl Pts',(1.86195461813654,0.116666666666666,-1.075));
#20049=CARTESIAN_POINT('Ctrl Pts',(2.48260615751539,0.174999999999999,-4.5604735265171E-16));
#20050=CARTESIAN_POINT('Ctrl Pts',(1.86195461813654,0.233333333333332,1.075));
#20051=CARTESIAN_POINT('Ctrl Pts',(1.2413030787577,0.291666666666665,2.15));
#20052=CARTESIAN_POINT('Ctrl Pts',(0.,0.349999999999999,2.15));
#20053=CARTESIAN_POINT('Ctrl Pts',(-1.2413030787577,0.408333333333332,2.15));
#20054=CARTESIAN_POINT('Ctrl Pts',(-1.86195461813654,0.466666666666665,
1.075));
#20055=CARTESIAN_POINT('Ctrl Pts',(-2.48260615751539,0.524999999999998,
1.52015784217237E-16));
#20056=CARTESIAN_POINT('Ctrl Pts',(-1.86195461813654,0.583333333333331,
-1.075));
#20057=CARTESIAN_POINT('Ctrl Pts',(-1.2413030787577,0.641666666666665,-2.15));
#20058=CARTESIAN_POINT('Ctrl Pts',(-2.63299061816681E-16,0.699999999999998,
-2.15));
#20059=CARTESIAN_POINT('Ctrl Pts',(1.24130307875769,0.758333333333331,-2.15));
#20060=CARTESIAN_POINT('Ctrl Pts',(1.86195461813654,0.816666666666664,-1.075));
#20061=CARTESIAN_POINT('Ctrl Pts',(2.48260615751539,0.874999999999997,-4.5604735265171E-16));
#20062=CARTESIAN_POINT('Ctrl Pts',(1.86195461813654,0.933333333333331,1.075));
#20063=CARTESIAN_POINT('Ctrl Pts',(1.2413030787577,0.991666666666664,2.15));
#20064=CARTESIAN_POINT('Ctrl Pts',(0.,1.05,2.15));
#20065=CARTESIAN_POINT('Ctrl Pts',(-1.2413030787577,1.10833333333333,2.15));
#20066=CARTESIAN_POINT('Ctrl Pts',(-1.86195461813654,1.16666666666666,1.075));
#20067=CARTESIAN_POINT('Ctrl Pts',(-2.48260615751539,1.225,1.52015784217237E-16));
#20068=CARTESIAN_POINT('Ctrl Pts',(-1.86195461813654,1.28333333333333,-1.075));
#20069=CARTESIAN_POINT('Ctrl Pts',(-1.2413030787577,1.34166666666666,-2.15));
#20070=CARTESIAN_POINT('Ctrl Pts',(-2.63299061816681E-16,1.4,-2.15));
#20071=CARTESIAN_POINT('Ctrl Pts',(1.24130307875769,1.45833333333333,-2.15));
#20072=CARTESIAN_POINT('Ctrl Pts',(1.86195461813654,1.51666666666666,-1.075));
#20073=CARTESIAN_POINT('Ctrl Pts',(2.48260615751539,1.575,-4.5604735265171E-16));
#20074=CARTESIAN_POINT('Ctrl Pts',(1.86195461813654,1.63333333333333,1.075));
#20075=CARTESIAN_POINT('Ctrl Pts',(1.2413030787577,1.69166666666666,2.15));
#20076=CARTESIAN_POINT('Ctrl Pts',(0.,1.75,2.15));
#20077=CARTESIAN_POINT('Ctrl Pts',(-1.2413030787577,1.80833333333333,2.15));
#20078=CARTESIAN_POINT('Ctrl Pts',(-1.86195461813654,1.86666666666666,1.075));
#20079=CARTESIAN_POINT('Ctrl Pts',(-2.48260615751539,1.925,1.52015784217237E-16));
#20080=CARTESIAN_POINT('Ctrl Pts',(-1.86195461813654,1.98333333333333,-1.075));
#20081=CARTESIAN_POINT('Ctrl Pts',(-1.2413030787577,2.04166666666666,-2.15));
#20082=CARTESIAN_POINT('Ctrl Pts',(-2.63299061816681E-16,2.1,-2.15));
#20083=CARTESIAN_POINT('Ctrl Pts',(1.24130307875769,2.15833333333333,-2.15));
#20084=CARTESIAN_POINT('Ctrl Pts',(1.86195461813654,2.21666666666666,-1.075));
#20085=CARTESIAN_POINT('Ctrl Pts',(2.48260615751539,2.275,-4.5604735265171E-16));
#20086=CARTESIAN_POINT('Ctrl Pts',(1.86195461813654,2.33333333333333,1.075));
#20087=CARTESIAN_POINT('Ctrl Pts',(1.2413030787577,2.39166666666666,2.15));
#20088=CARTESIAN_POINT('Ctrl Pts',(0.,2.44999999999999,2.15));
#20089=CARTESIAN_POINT('Ctrl Pts',(-1.2413030787577,2.50833333333333,2.15));
#20090=CARTESIAN_POINT('Ctrl Pts',(-1.86195461813654,2.56666666666666,1.075));
#20091=CARTESIAN_POINT('Ctrl Pts',(-2.48260615751539,2.62499999999999,1.52015784217237E-16));
#20092=CARTESIAN_POINT('Ctrl Pts',(-1.86195461813654,2.68333333333333,-1.075));
#20093=CARTESIAN_POINT('Ctrl Pts',(-1.2413030787577,2.74166666666666,-2.15));
#20094=CARTESIAN_POINT('Ctrl Pts',(-2.63299061816681E-16,2.79999999999999,
-2.15));
#20095=CARTESIAN_POINT('Ctrl Pts',(1.24130307875769,2.85833333333333,-2.15));
#20096=CARTESIAN_POINT('Ctrl Pts',(1.86195461813654,2.91666666666666,-1.075));
#20097=CARTESIAN_POINT('Ctrl Pts',(2.48260615751539,2.97499999999999,-4.5604735265171E-16));
#20098=CARTESIAN_POINT('Ctrl Pts',(1.86195461813654,3.03333333333333,1.075));
#20099=CARTESIAN_POINT('Ctrl Pts',(1.2413030787577,3.09166666666666,2.15));
#20100=CARTESIAN_POINT('Ctrl Pts',(0.,3.14999999999999,2.15));
#20101=CARTESIAN_POINT('Ctrl Pts',(-1.2413030787577,3.20833333333333,2.15));
#20102=CARTESIAN_POINT('Ctrl Pts',(-1.86195461813654,3.26666666666666,1.075));
#20103=CARTESIAN_POINT('Ctrl Pts',(-2.48260615751539,3.32499999999999,1.52015784217237E-16));
#20104=CARTESIAN_POINT('Ctrl Pts',(-1.86195461813654,3.38333333333333,-1.075));
#20105=CARTESIAN_POINT('Ctrl Pts',(-1.2413030787577,3.44166666666666,-2.15));
#20106=CARTESIAN_POINT('Ctrl Pts',(-2.63299061816681E-16,3.49999999999999,
-2.15));
#20107=CARTESIAN_POINT('Ctrl Pts',(1.24130307875769,3.55833333333333,-2.15));
#20108=CARTESIAN_POINT('Ctrl Pts',(1.86195461813654,3.61666666666666,-1.075));
#20109=CARTESIAN_POINT('Ctrl Pts',(2.48260615751539,3.67499999999999,-4.5604735265171E-16));
#20110=CARTESIAN_POINT('Ctrl Pts',(1.86195461813654,3.73333333333333,1.075));
#20111=CARTESIAN_POINT('Ctrl Pts',(1.2413030787577,3.79166666666666,2.15));
#20112=CARTESIAN_POINT('Ctrl Pts',(0.,3.84999999999999,2.15));
#20113=CARTESIAN_POINT('Ctrl Pts',(0.,-0.35,1.94497474683058));
#20114=CARTESIAN_POINT('Ctrl Pts',(-1.12293169364966,-0.291666666666667,
1.94497474683058));
#20115=CARTESIAN_POINT('Ctrl Pts',(-1.68439754047449,-0.233333333333334,
0.972487373415292));
#20116=CARTESIAN_POINT('Ctrl Pts',(-2.24586338729932,-0.175,1.37519470428917E-16));
#20117=CARTESIAN_POINT('Ctrl Pts',(-1.68439754047449,-0.116666666666667,
-0.972487373415291));
#20118=CARTESIAN_POINT('Ctrl Pts',(-1.12293169364966,-0.058333333333334,
-1.94497474683058));
#20119=CARTESIAN_POINT('Ctrl Pts',(-2.38190709812851E-16,-8.13151629364128E-16,
-1.94497474683058));
#20120=CARTESIAN_POINT('Ctrl Pts',(1.12293169364966,0.0583333333333324,
-1.94497474683058));
#20121=CARTESIAN_POINT('Ctrl Pts',(1.68439754047449,0.116666666666666,-0.972487373415292));
#20122=CARTESIAN_POINT('Ctrl Pts',(2.24586338729932,0.174999999999999,-4.12558411286752E-16));
#20123=CARTESIAN_POINT('Ctrl Pts',(1.68439754047449,0.233333333333332,0.97248737341529));
#20124=CARTESIAN_POINT('Ctrl Pts',(1.12293169364966,0.291666666666665,1.94497474683058));
#20125=CARTESIAN_POINT('Ctrl Pts',(0.,0.349999999999998,1.94497474683058));
#20126=CARTESIAN_POINT('Ctrl Pts',(-1.12293169364966,0.408333333333332,
1.94497474683058));
#20127=CARTESIAN_POINT('Ctrl Pts',(-1.68439754047449,0.466666666666665,
0.972487373415292));
#20128=CARTESIAN_POINT('Ctrl Pts',(-2.24586338729932,0.524999999999998,
1.37519470428917E-16));
#20129=CARTESIAN_POINT('Ctrl Pts',(-1.68439754047449,0.583333333333331,
-0.972487373415291));
#20130=CARTESIAN_POINT('Ctrl Pts',(-1.12293169364966,0.641666666666665,
-1.94497474683058));
#20131=CARTESIAN_POINT('Ctrl Pts',(-2.38190709812851E-16,0.699999999999998,
-1.94497474683058));
#20132=CARTESIAN_POINT('Ctrl Pts',(1.12293169364966,0.758333333333331,-1.94497474683058));
#20133=CARTESIAN_POINT('Ctrl Pts',(1.68439754047449,0.816666666666664,-0.972487373415292));
#20134=CARTESIAN_POINT('Ctrl Pts',(2.24586338729932,0.874999999999998,-4.12558411286752E-16));
#20135=CARTESIAN_POINT('Ctrl Pts',(1.68439754047449,0.933333333333331,0.97248737341529));
#20136=CARTESIAN_POINT('Ctrl Pts',(1.12293169364966,0.991666666666664,1.94497474683058));
#20137=CARTESIAN_POINT('Ctrl Pts',(0.,1.05,1.94497474683058));
#20138=CARTESIAN_POINT('Ctrl Pts',(-1.12293169364966,1.10833333333333,1.94497474683058));
#20139=CARTESIAN_POINT('Ctrl Pts',(-1.68439754047449,1.16666666666666,0.972487373415292));
#20140=CARTESIAN_POINT('Ctrl Pts',(-2.24586338729932,1.225,1.37519470428917E-16));
#20141=CARTESIAN_POINT('Ctrl Pts',(-1.68439754047449,1.28333333333333,-0.972487373415291));
#20142=CARTESIAN_POINT('Ctrl Pts',(-1.12293169364966,1.34166666666666,-1.94497474683058));
#20143=CARTESIAN_POINT('Ctrl Pts',(-2.38190709812851E-16,1.4,-1.94497474683058));
#20144=CARTESIAN_POINT('Ctrl Pts',(1.12293169364966,1.45833333333333,-1.94497474683058));
#20145=CARTESIAN_POINT('Ctrl Pts',(1.68439754047449,1.51666666666666,-0.972487373415292));
#20146=CARTESIAN_POINT('Ctrl Pts',(2.24586338729932,1.575,-4.12558411286752E-16));
#20147=CARTESIAN_POINT('Ctrl Pts',(1.68439754047449,1.63333333333333,0.97248737341529));
#20148=CARTESIAN_POINT('Ctrl Pts',(1.12293169364966,1.69166666666666,1.94497474683058));
#20149=CARTESIAN_POINT('Ctrl Pts',(0.,1.75,1.94497474683058));
#20150=CARTESIAN_POINT('Ctrl Pts',(-1.12293169364966,1.80833333333333,1.94497474683058));
#20151=CARTESIAN_POINT('Ctrl Pts',(-1.68439754047449,1.86666666666666,0.972487373415292));
#20152=CARTESIAN_POINT('Ctrl Pts',(-2.24586338729932,1.925,1.37519470428917E-16));
#20153=CARTESIAN_POINT('Ctrl Pts',(-1.68439754047449,1.98333333333333,-0.972487373415291));
#20154=CARTESIAN_POINT('Ctrl Pts',(-1.12293169364966,2.04166666666666,-1.94497474683058));
#20155=CARTESIAN_POINT('Ctrl Pts',(-2.38190709812851E-16,2.09999999999999,
-1.94497474683058));
#20156=CARTESIAN_POINT('Ctrl Pts',(1.12293169364966,2.15833333333333,-1.94497474683058));
#20157=CARTESIAN_POINT('Ctrl Pts',(1.68439754047449,2.21666666666666,-0.972487373415292));
#20158=CARTESIAN_POINT('Ctrl Pts',(2.24586338729932,2.275,-4.12558411286752E-16));
#20159=CARTESIAN_POINT('Ctrl Pts',(1.68439754047449,2.33333333333333,0.97248737341529));
#20160=CARTESIAN_POINT('Ctrl Pts',(1.12293169364966,2.39166666666666,1.94497474683058));
#20161=CARTESIAN_POINT('Ctrl Pts',(0.,2.44999999999999,1.94497474683058));
#20162=CARTESIAN_POINT('Ctrl Pts',(-1.12293169364966,2.50833333333333,1.94497474683058));
#20163=CARTESIAN_POINT('Ctrl Pts',(-1.68439754047449,2.56666666666666,0.972487373415292));
#20164=CARTESIAN_POINT('Ctrl Pts',(-2.24586338729932,2.62499999999999,1.37519470428917E-16));
#20165=CARTESIAN_POINT('Ctrl Pts',(-1.68439754047449,2.68333333333333,-0.972487373415291));
#20166=CARTESIAN_POINT('Ctrl Pts',(-1.12293169364966,2.74166666666666,-1.94497474683058));
#20167=CARTESIAN_POINT('Ctrl Pts',(-2.38190709812851E-16,2.79999999999999,
-1.94497474683058));
#20168=CARTESIAN_POINT('Ctrl Pts',(1.12293169364966,2.85833333333333,-1.94497474683058));
#20169=CARTESIAN_POINT('Ctrl Pts',(1.68439754047449,2.91666666666666,-0.972487373415292));
#20170=CARTESIAN_POINT('Ctrl Pts',(2.24586338729932,2.97499999999999,-4.12558411286752E-16));
#20171=CARTESIAN_POINT('Ctrl Pts',(1.68439754047449,3.03333333333333,0.97248737341529));
#20172=CARTESIAN_POINT('Ctrl Pts',(1.12293169364966,3.09166666666666,1.94497474683058));
#20173=CARTESIAN_POINT('Ctrl Pts',(0.,3.14999999999999,1.94497474683058));
#20174=CARTESIAN_POINT('Ctrl Pts',(-1.12293169364966,3.20833333333333,1.94497474683058));
#20175=CARTESIAN_POINT('Ctrl Pts',(-1.68439754047449,3.26666666666666,0.972487373415292));
#20176=CARTESIAN_POINT('Ctrl Pts',(-2.24586338729932,3.32499999999999,1.37519470428917E-16));
#20177=CARTESIAN_POINT('Ctrl Pts',(-1.68439754047449,3.38333333333333,-0.972487373415291));
#20178=CARTESIAN_POINT('Ctrl Pts',(-1.12293169364966,3.44166666666666,-1.94497474683058));
#20179=CARTESIAN_POINT('Ctrl Pts',(-2.38190709812851E-16,3.49999999999999,
-1.94497474683058));
#20180=CARTESIAN_POINT('Ctrl Pts',(1.12293169364966,3.55833333333333,-1.94497474683058));
#20181=CARTESIAN_POINT('Ctrl Pts',(1.68439754047449,3.61666666666666,-0.972487373415292));
#20182=CARTESIAN_POINT('Ctrl Pts',(2.24586338729932,3.67499999999999,-4.12558411286752E-16));
#20183=CARTESIAN_POINT('Ctrl Pts',(1.68439754047449,3.73333333333332,0.97248737341529));
#20184=CARTESIAN_POINT('Ctrl Pts',(1.12293169364966,3.79166666666666,1.94497474683058));
#20185=CARTESIAN_POINT('Ctrl Pts',(0.,3.84999999999999,1.94497474683058));
#20186=CARTESIAN_POINT('Ctrl Pts',(0.,-0.205025253169417,1.8));
#20187=CARTESIAN_POINT('Ctrl Pts',(-1.03923048454133,-0.146691919836083,
1.8));
#20188=CARTESIAN_POINT('Ctrl Pts',(-1.55884572681199,-0.0883585865027503,
0.9));
#20189=CARTESIAN_POINT('Ctrl Pts',(-2.07846096908265,-0.0300252531694171,
1.27269028646989E-16));
#20190=CARTESIAN_POINT('Ctrl Pts',(-1.55884572681199,0.0283080801639161,
-0.9));
#20191=CARTESIAN_POINT('Ctrl Pts',(-1.03923048454133,0.0866414134972494,
-1.8));
#20192=CARTESIAN_POINT('Ctrl Pts',(-2.20436423846524E-16,0.144974746830583,
-1.8));
#20193=CARTESIAN_POINT('Ctrl Pts',(1.03923048454133,0.203308080163916,-1.8));
#20194=CARTESIAN_POINT('Ctrl Pts',(1.55884572681199,0.261641413497249,-0.900000000000001));
#20195=CARTESIAN_POINT('Ctrl Pts',(2.07846096908265,0.319974746830582,-3.81807085940967E-16));
#20196=CARTESIAN_POINT('Ctrl Pts',(1.55884572681199,0.378308080163915,0.899999999999999));
#20197=CARTESIAN_POINT('Ctrl Pts',(1.03923048454133,0.436641413497249,1.8));
#20198=CARTESIAN_POINT('Ctrl Pts',(0.,0.494974746830582,1.8));
#20199=CARTESIAN_POINT('Ctrl Pts',(-1.03923048454133,0.553308080163915,
1.8));
#20200=CARTESIAN_POINT('Ctrl Pts',(-1.55884572681199,0.611641413497248,
0.9));
#20201=CARTESIAN_POINT('Ctrl Pts',(-2.07846096908265,0.669974746830582,
1.27269028646989E-16));
#20202=CARTESIAN_POINT('Ctrl Pts',(-1.55884572681199,0.728308080163915,
-0.9));
#20203=CARTESIAN_POINT('Ctrl Pts',(-1.03923048454133,0.786641413497248,
-1.8));
#20204=CARTESIAN_POINT('Ctrl Pts',(-2.20436423846524E-16,0.844974746830581,
-1.8));
#20205=CARTESIAN_POINT('Ctrl Pts',(1.03923048454133,0.903308080163914,-1.8));
#20206=CARTESIAN_POINT('Ctrl Pts',(1.55884572681199,0.961641413497248,-0.900000000000001));
#20207=CARTESIAN_POINT('Ctrl Pts',(2.07846096908265,1.01997474683058,-3.81807085940967E-16));
#20208=CARTESIAN_POINT('Ctrl Pts',(1.55884572681199,1.07830808016391,0.899999999999999));
#20209=CARTESIAN_POINT('Ctrl Pts',(1.03923048454133,1.13664141349725,1.8));
#20210=CARTESIAN_POINT('Ctrl Pts',(0.,1.19497474683058,1.8));
#20211=CARTESIAN_POINT('Ctrl Pts',(-1.03923048454133,1.25330808016391,1.8));
#20212=CARTESIAN_POINT('Ctrl Pts',(-1.55884572681199,1.31164141349725,0.9));
#20213=CARTESIAN_POINT('Ctrl Pts',(-2.07846096908265,1.36997474683058,1.27269028646989E-16));
#20214=CARTESIAN_POINT('Ctrl Pts',(-1.55884572681199,1.42830808016391,-0.9));
#20215=CARTESIAN_POINT('Ctrl Pts',(-1.03923048454133,1.48664141349725,-1.8));
#20216=CARTESIAN_POINT('Ctrl Pts',(-2.20436423846524E-16,1.54497474683058,
-1.8));
#20217=CARTESIAN_POINT('Ctrl Pts',(1.03923048454133,1.60330808016391,-1.8));
#20218=CARTESIAN_POINT('Ctrl Pts',(1.55884572681199,1.66164141349725,-0.900000000000001));
#20219=CARTESIAN_POINT('Ctrl Pts',(2.07846096908265,1.71997474683058,-3.81807085940967E-16));
#20220=CARTESIAN_POINT('Ctrl Pts',(1.55884572681199,1.77830808016391,0.899999999999999));
#20221=CARTESIAN_POINT('Ctrl Pts',(1.03923048454133,1.83664141349725,1.8));
#20222=CARTESIAN_POINT('Ctrl Pts',(0.,1.89497474683058,1.8));
#20223=CARTESIAN_POINT('Ctrl Pts',(-1.03923048454133,1.95330808016391,1.8));
#20224=CARTESIAN_POINT('Ctrl Pts',(-1.55884572681199,2.01164141349725,0.9));
#20225=CARTESIAN_POINT('Ctrl Pts',(-2.07846096908265,2.06997474683058,1.27269028646989E-16));
#20226=CARTESIAN_POINT('Ctrl Pts',(-1.55884572681199,2.12830808016391,-0.9));
#20227=CARTESIAN_POINT('Ctrl Pts',(-1.03923048454133,2.18664141349725,-1.8));
#20228=CARTESIAN_POINT('Ctrl Pts',(-2.20436423846524E-16,2.24497474683058,
-1.8));
#20229=CARTESIAN_POINT('Ctrl Pts',(1.03923048454133,2.30330808016391,-1.8));
#20230=CARTESIAN_POINT('Ctrl Pts',(1.55884572681199,2.36164141349724,-0.900000000000001));
#20231=CARTESIAN_POINT('Ctrl Pts',(2.07846096908265,2.41997474683058,-3.81807085940967E-16));
#20232=CARTESIAN_POINT('Ctrl Pts',(1.55884572681199,2.47830808016391,0.899999999999999));
#20233=CARTESIAN_POINT('Ctrl Pts',(1.03923048454133,2.53664141349724,1.8));
#20234=CARTESIAN_POINT('Ctrl Pts',(0.,2.59497474683058,1.8));
#20235=CARTESIAN_POINT('Ctrl Pts',(-1.03923048454133,2.65330808016391,1.8));
#20236=CARTESIAN_POINT('Ctrl Pts',(-1.55884572681199,2.71164141349724,0.9));
#20237=CARTESIAN_POINT('Ctrl Pts',(-2.07846096908265,2.76997474683058,1.27269028646989E-16));
#20238=CARTESIAN_POINT('Ctrl Pts',(-1.55884572681199,2.82830808016391,-0.9));
#20239=CARTESIAN_POINT('Ctrl Pts',(-1.03923048454133,2.88664141349724,-1.8));
#20240=CARTESIAN_POINT('Ctrl Pts',(-2.20436423846524E-16,2.94497474683058,
-1.8));
#20241=CARTESIAN_POINT('Ctrl Pts',(1.03923048454133,3.00330808016391,-1.8));
#20242=CARTESIAN_POINT('Ctrl Pts',(1.55884572681199,3.06164141349724,-0.900000000000001));
#20243=CARTESIAN_POINT('Ctrl Pts',(2.07846096908265,3.11997474683058,-3.81807085940967E-16));
#20244=CARTESIAN_POINT('Ctrl Pts',(1.55884572681199,3.17830808016391,0.899999999999999));
#20245=CARTESIAN_POINT('Ctrl Pts',(1.03923048454133,3.23664141349724,1.8));
#20246=CARTESIAN_POINT('Ctrl Pts',(0.,3.29497474683058,1.8));
#20247=CARTESIAN_POINT('Ctrl Pts',(-1.03923048454133,3.35330808016391,1.8));
#20248=CARTESIAN_POINT('Ctrl Pts',(-1.55884572681199,3.41164141349724,0.9));
#20249=CARTESIAN_POINT('Ctrl Pts',(-2.07846096908265,3.46997474683058,1.27269028646989E-16));
#20250=CARTESIAN_POINT('Ctrl Pts',(-1.55884572681199,3.52830808016391,-0.9));
#20251=CARTESIAN_POINT('Ctrl Pts',(-1.03923048454133,3.58664141349724,-1.8));
#20252=CARTESIAN_POINT('Ctrl Pts',(-2.20436423846524E-16,3.64497474683058,
-1.8));
#20253=CARTESIAN_POINT('Ctrl Pts',(1.03923048454133,3.70330808016391,-1.8));
#20254=CARTESIAN_POINT('Ctrl Pts',(1.55884572681199,3.76164141349724,-0.900000000000001));
#20255=CARTESIAN_POINT('Ctrl Pts',(2.07846096908265,3.81997474683058,-3.81807085940967E-16));
#20256=CARTESIAN_POINT('Ctrl Pts',(1.55884572681199,3.87830808016391,0.899999999999999));
#20257=CARTESIAN_POINT('Ctrl Pts',(1.03923048454133,3.93664141349724,1.8));
#20258=CARTESIAN_POINT('Ctrl Pts',(0.,3.99497474683058,1.8));
#20259=CARTESIAN_POINT('Ctrl Pts',(0.,0.,1.8));
#20260=CARTESIAN_POINT('Ctrl Pts',(-1.03923048454133,0.0583333333333332,
1.8));
#20261=CARTESIAN_POINT('Ctrl Pts',(-1.55884572681199,0.116666666666666,
0.9));
#20262=CARTESIAN_POINT('Ctrl Pts',(-2.07846096908265,0.175,1.27269028646989E-16));
#20263=CARTESIAN_POINT('Ctrl Pts',(-1.55884572681199,0.233333333333333,
-0.9));
#20264=CARTESIAN_POINT('Ctrl Pts',(-1.03923048454133,0.291666666666666,
-1.8));
#20265=CARTESIAN_POINT('Ctrl Pts',(-2.20436423846524E-16,0.349999999999999,
-1.8));
#20266=CARTESIAN_POINT('Ctrl Pts',(1.03923048454133,0.408333333333333,-1.8));
#20267=CARTESIAN_POINT('Ctrl Pts',(1.55884572681199,0.466666666666666,-0.900000000000001));
#20268=CARTESIAN_POINT('Ctrl Pts',(2.07846096908265,0.524999999999999,-3.81807085940967E-16));
#20269=CARTESIAN_POINT('Ctrl Pts',(1.55884572681199,0.583333333333332,0.899999999999999));
#20270=CARTESIAN_POINT('Ctrl Pts',(1.03923048454133,0.641666666666665,1.8));
#20271=CARTESIAN_POINT('Ctrl Pts',(0.,0.699999999999999,1.8));
#20272=CARTESIAN_POINT('Ctrl Pts',(-1.03923048454133,0.758333333333332,
1.8));
#20273=CARTESIAN_POINT('Ctrl Pts',(-1.55884572681199,0.816666666666665,
0.9));
#20274=CARTESIAN_POINT('Ctrl Pts',(-2.07846096908265,0.874999999999998,
1.27269028646989E-16));
#20275=CARTESIAN_POINT('Ctrl Pts',(-1.55884572681199,0.933333333333332,
-0.9));
#20276=CARTESIAN_POINT('Ctrl Pts',(-1.03923048454133,0.991666666666665,
-1.8));
#20277=CARTESIAN_POINT('Ctrl Pts',(-2.20436423846524E-16,1.05,-1.8));
#20278=CARTESIAN_POINT('Ctrl Pts',(1.03923048454133,1.10833333333333,-1.8));
#20279=CARTESIAN_POINT('Ctrl Pts',(1.55884572681199,1.16666666666666,-0.900000000000001));
#20280=CARTESIAN_POINT('Ctrl Pts',(2.07846096908265,1.225,-3.81807085940967E-16));
#20281=CARTESIAN_POINT('Ctrl Pts',(1.55884572681199,1.28333333333333,0.899999999999999));
#20282=CARTESIAN_POINT('Ctrl Pts',(1.03923048454133,1.34166666666666,1.8));
#20283=CARTESIAN_POINT('Ctrl Pts',(0.,1.4,1.8));
#20284=CARTESIAN_POINT('Ctrl Pts',(-1.03923048454133,1.45833333333333,1.8));
#20285=CARTESIAN_POINT('Ctrl Pts',(-1.55884572681199,1.51666666666666,0.9));
#20286=CARTESIAN_POINT('Ctrl Pts',(-2.07846096908265,1.575,1.27269028646989E-16));
#20287=CARTESIAN_POINT('Ctrl Pts',(-1.55884572681199,1.63333333333333,-0.9));
#20288=CARTESIAN_POINT('Ctrl Pts',(-1.03923048454133,1.69166666666666,-1.8));
#20289=CARTESIAN_POINT('Ctrl Pts',(-2.20436423846524E-16,1.75,-1.8));
#20290=CARTESIAN_POINT('Ctrl Pts',(1.03923048454133,1.80833333333333,-1.8));
#20291=CARTESIAN_POINT('Ctrl Pts',(1.55884572681199,1.86666666666666,-0.900000000000001));
#20292=CARTESIAN_POINT('Ctrl Pts',(2.07846096908265,1.925,-3.81807085940967E-16));
#20293=CARTESIAN_POINT('Ctrl Pts',(1.55884572681199,1.98333333333333,0.899999999999999));
#20294=CARTESIAN_POINT('Ctrl Pts',(1.03923048454133,2.04166666666666,1.8));
#20295=CARTESIAN_POINT('Ctrl Pts',(0.,2.1,1.8));
#20296=CARTESIAN_POINT('Ctrl Pts',(-1.03923048454133,2.15833333333333,1.8));
#20297=CARTESIAN_POINT('Ctrl Pts',(-1.55884572681199,2.21666666666666,0.9));
#20298=CARTESIAN_POINT('Ctrl Pts',(-2.07846096908265,2.275,1.27269028646989E-16));
#20299=CARTESIAN_POINT('Ctrl Pts',(-1.55884572681199,2.33333333333333,-0.9));
#20300=CARTESIAN_POINT('Ctrl Pts',(-1.03923048454133,2.39166666666666,-1.8));
#20301=CARTESIAN_POINT('Ctrl Pts',(-2.20436423846524E-16,2.45,-1.8));
#20302=CARTESIAN_POINT('Ctrl Pts',(1.03923048454133,2.50833333333333,-1.8));
#20303=CARTESIAN_POINT('Ctrl Pts',(1.55884572681199,2.56666666666666,-0.900000000000001));
#20304=CARTESIAN_POINT('Ctrl Pts',(2.07846096908265,2.62499999999999,-3.81807085940967E-16));
#20305=CARTESIAN_POINT('Ctrl Pts',(1.55884572681199,2.68333333333333,0.899999999999999));
#20306=CARTESIAN_POINT('Ctrl Pts',(1.03923048454133,2.74166666666666,1.8));
#20307=CARTESIAN_POINT('Ctrl Pts',(0.,2.79999999999999,1.8));
#20308=CARTESIAN_POINT('Ctrl Pts',(-1.03923048454133,2.85833333333333,1.8));
#20309=CARTESIAN_POINT('Ctrl Pts',(-1.55884572681199,2.91666666666666,0.9));
#20310=CARTESIAN_POINT('Ctrl Pts',(-2.07846096908265,2.97499999999999,1.27269028646989E-16));
#20311=CARTESIAN_POINT('Ctrl Pts',(-1.55884572681199,3.03333333333333,-0.9));
#20312=CARTESIAN_POINT('Ctrl Pts',(-1.03923048454133,3.09166666666666,-1.8));
#20313=CARTESIAN_POINT('Ctrl Pts',(-2.20436423846524E-16,3.14999999999999,
-1.8));
#20314=CARTESIAN_POINT('Ctrl Pts',(1.03923048454133,3.20833333333333,-1.8));
#20315=CARTESIAN_POINT('Ctrl Pts',(1.55884572681199,3.26666666666666,-0.900000000000001));
#20316=CARTESIAN_POINT('Ctrl Pts',(2.07846096908265,3.32499999999999,-3.81807085940967E-16));
#20317=CARTESIAN_POINT('Ctrl Pts',(1.55884572681199,3.38333333333333,0.899999999999999));
#20318=CARTESIAN_POINT('Ctrl Pts',(1.03923048454133,3.44166666666666,1.8));
#20319=CARTESIAN_POINT('Ctrl Pts',(0.,3.49999999999999,1.8));
#20320=CARTESIAN_POINT('Ctrl Pts',(-1.03923048454133,3.55833333333333,1.8));
#20321=CARTESIAN_POINT('Ctrl Pts',(-1.55884572681199,3.61666666666666,0.9));
#20322=CARTESIAN_POINT('Ctrl Pts',(-2.07846096908265,3.67499999999999,1.27269028646989E-16));
#20323=CARTESIAN_POINT('Ctrl Pts',(-1.55884572681199,3.73333333333333,-0.9));
#20324=CARTESIAN_POINT('Ctrl Pts',(-1.03923048454133,3.79166666666666,-1.8));
#20325=CARTESIAN_POINT('Ctrl Pts',(-2.20436423846524E-16,3.84999999999999,
-1.8));
#20326=CARTESIAN_POINT('Ctrl Pts',(1.03923048454133,3.90833333333333,-1.8));
#20327=CARTESIAN_POINT('Ctrl Pts',(1.55884572681199,3.96666666666666,-0.900000000000001));
#20328=CARTESIAN_POINT('Ctrl Pts',(2.07846096908265,4.02499999999999,-3.81807085940967E-16));
#20329=CARTESIAN_POINT('Ctrl Pts',(1.55884572681199,4.08333333333333,0.899999999999999));
#20330=CARTESIAN_POINT('Ctrl Pts',(1.03923048454133,4.14166666666666,1.8));
#20331=CARTESIAN_POINT('Ctrl Pts',(0.,4.19999999999999,1.8));
#20332=CARTESIAN_POINT('',(-2.63299061816681E-16,-0.349999999999999,2.15));
#20333=CARTESIAN_POINT('Origin',(0.,0.,2.15));
#20334=CARTESIAN_POINT('Ctrl Pts',(-2.63299061816681E-16,-0.349999999999999,
2.15));
#20335=CARTESIAN_POINT('Ctrl Pts',(-1.2413030787577,-0.291666666666666,
2.15));
#20336=CARTESIAN_POINT('Ctrl Pts',(-1.86195461813654,-0.233333333333333,
1.075));
#20337=CARTESIAN_POINT('Ctrl Pts',(-2.48260615751539,-0.175,-1.52015784217237E-16));
#20338=CARTESIAN_POINT('Ctrl Pts',(-1.86195461813654,-0.116666666666666,
-1.075));
#20339=CARTESIAN_POINT('Ctrl Pts',(-1.2413030787577,-0.0583333333333332,
-2.15));
#20340=CARTESIAN_POINT('Ctrl Pts',(0.,0.,-2.15));
#20341=CARTESIAN_POINT('Ctrl Pts',(1.24130307875769,0.0583333333333333,
-2.15));
#20342=CARTESIAN_POINT('Ctrl Pts',(1.86195461813654,0.116666666666666,-1.075));
#20343=CARTESIAN_POINT('Ctrl Pts',(2.48260615751539,0.175,-1.52015784217237E-16));
#20344=CARTESIAN_POINT('Ctrl Pts',(1.86195461813654,0.233333333333333,1.075));
#20345=CARTESIAN_POINT('Ctrl Pts',(1.2413030787577,0.291666666666666,2.15));
#20346=CARTESIAN_POINT('Ctrl Pts',(2.63299061816681E-16,0.349999999999999,
2.15));
#20347=CARTESIAN_POINT('Ctrl Pts',(2.63299061816681E-16,0.349999999999999,
2.15));
#20348=CARTESIAN_POINT('Ctrl Pts',(-1.24130307875769,0.408333333333333,
2.15));
#20349=CARTESIAN_POINT('Ctrl Pts',(-1.86195461813654,0.466666666666666,
1.075));
#20350=CARTESIAN_POINT('Ctrl Pts',(-2.48260615751539,0.524999999999999,
4.5604735265171E-16));
#20351=CARTESIAN_POINT('Ctrl Pts',(-1.86195461813654,0.583333333333332,
-1.075));
#20352=CARTESIAN_POINT('Ctrl Pts',(-1.2413030787577,0.641666666666665,-2.15));
#20353=CARTESIAN_POINT('Ctrl Pts',(-5.26598123633362E-16,0.699999999999999,
-2.15));
#20354=CARTESIAN_POINT('Ctrl Pts',(1.24130307875769,0.758333333333332,-2.15));
#20355=CARTESIAN_POINT('Ctrl Pts',(1.86195461813654,0.816666666666665,-1.075));
#20356=CARTESIAN_POINT('Ctrl Pts',(2.48260615751539,0.874999999999999,-7.60078921086183E-16));
#20357=CARTESIAN_POINT('Ctrl Pts',(1.86195461813654,0.933333333333332,1.075));
#20358=CARTESIAN_POINT('Ctrl Pts',(1.2413030787577,0.991666666666665,2.15));
#20359=CARTESIAN_POINT('Ctrl Pts',(7.89897185450043E-16,1.05,2.15));
#20360=CARTESIAN_POINT('Ctrl Pts',(-1.24130307875769,1.10833333333333,2.15));
#20361=CARTESIAN_POINT('Ctrl Pts',(-1.86195461813654,1.16666666666666,1.075));
#20362=CARTESIAN_POINT('Ctrl Pts',(-2.48260615751539,1.225,3.26910770324048E-15));
#20363=CARTESIAN_POINT('Ctrl Pts',(-1.86195461813654,1.28333333333333,-1.075));
#20364=CARTESIAN_POINT('Ctrl Pts',(-1.2413030787577,1.34166666666666,-2.15));
#20365=CARTESIAN_POINT('Ctrl Pts',(-1.05319624726672E-15,1.4,-2.15));
#20366=CARTESIAN_POINT('Ctrl Pts',(1.24130307875769,1.45833333333333,-2.15));
#20367=CARTESIAN_POINT('Ctrl Pts',(1.86195461813654,1.51666666666666,-1.075));
#20368=CARTESIAN_POINT('Ctrl Pts',(2.48260615751539,1.575,-1.36814205795513E-15));
#20369=CARTESIAN_POINT('Ctrl Pts',(1.86195461813654,1.63333333333333,1.075));
#20370=CARTESIAN_POINT('Ctrl Pts',(1.2413030787577,1.69166666666666,2.15));
#20371=CARTESIAN_POINT('Ctrl Pts',(1.3164953090834E-15,1.75,2.15));
#20372=CARTESIAN_POINT('Ctrl Pts',(-1.24130307875769,1.80833333333333,2.15));
#20373=CARTESIAN_POINT('Ctrl Pts',(-1.86195461813654,1.86666666666666,1.075));
#20374=CARTESIAN_POINT('Ctrl Pts',(-2.48260615751539,1.925,6.08216805382924E-15));
#20375=CARTESIAN_POINT('Ctrl Pts',(-1.86195461813654,1.98333333333333,-1.075));
#20376=CARTESIAN_POINT('Ctrl Pts',(-1.2413030787577,2.04166666666666,-2.15));
#20377=CARTESIAN_POINT('Ctrl Pts',(-5.39896157561062E-15,2.1,-2.15));
#20378=CARTESIAN_POINT('Ctrl Pts',(1.24130307875769,2.15833333333333,-2.15));
#20379=CARTESIAN_POINT('Ctrl Pts',(1.86195461813654,2.21666666666666,-1.075));
#20380=CARTESIAN_POINT('Ctrl Pts',(2.48260615751539,2.275,-6.38619962226372E-15));
#20381=CARTESIAN_POINT('Ctrl Pts',(1.86195461813655,2.33333333333333,1.07499999999999));
#20382=CARTESIAN_POINT('Ctrl Pts',(1.2413030787577,2.39166666666666,2.15));
#20383=CARTESIAN_POINT('Ctrl Pts',(1.84309343271677E-15,2.45,2.15));
#20384=CARTESIAN_POINT('Ctrl Pts',(-1.24130307875769,2.50833333333333,2.15));
#20385=CARTESIAN_POINT('Ctrl Pts',(-1.86195461813654,2.56666666666666,1.075));
#20386=CARTESIAN_POINT('Ctrl Pts',(-2.48260615751539,2.62499999999999,6.69023119069819E-15));
#20387=CARTESIAN_POINT('Ctrl Pts',(-1.86195461813655,2.68333333333333,-1.07499999999999));
#20388=CARTESIAN_POINT('Ctrl Pts',(-1.2413030787577,2.74166666666666,-2.14999999999999));
#20389=CARTESIAN_POINT('Ctrl Pts',(-2.10639249453345E-15,2.79999999999999,
-2.15));
#20390=CARTESIAN_POINT('Ctrl Pts',(1.24130307875769,2.85833333333333,-2.15));
#20391=CARTESIAN_POINT('Ctrl Pts',(1.86195461813654,2.91666666666666,-1.075));
#20392=CARTESIAN_POINT('Ctrl Pts',(2.48260615751539,2.97499999999999,-6.99426275913266E-15));
#20393=CARTESIAN_POINT('Ctrl Pts',(1.86195461813655,3.03333333333333,1.07499999999999));
#20394=CARTESIAN_POINT('Ctrl Pts',(1.2413030787577,3.09166666666666,2.14999999999999));
#20395=CARTESIAN_POINT('Ctrl Pts',(2.36969155635013E-15,3.14999999999999,
2.15));
#20396=CARTESIAN_POINT('Ctrl Pts',(-1.24130307875769,3.20833333333333,2.15));
#20397=CARTESIAN_POINT('Ctrl Pts',(-1.86195461813654,3.26666666666666,1.075));
#20398=CARTESIAN_POINT('Ctrl Pts',(-2.48260615751539,3.32499999999999,7.29829432756713E-15));
#20399=CARTESIAN_POINT('Ctrl Pts',(-1.86195461813655,3.38333333333333,-1.07499999999999));
#20400=CARTESIAN_POINT('Ctrl Pts',(-1.2413030787577,3.44166666666666,-2.14999999999999));
#20401=CARTESIAN_POINT('Ctrl Pts',(-1.02713250275879E-14,3.49999999999999,
-2.15));
#20402=CARTESIAN_POINT('Ctrl Pts',(1.24130307875769,3.55833333333333,-2.15));
#20403=CARTESIAN_POINT('Ctrl Pts',(1.86195461813654,3.61666666666666,-1.075));
#20404=CARTESIAN_POINT('Ctrl Pts',(2.48260615751539,3.67499999999999,-7.60232589600161E-15));
#20405=CARTESIAN_POINT('Ctrl Pts',(1.86195461813655,3.73333333333333,1.07499999999999));
#20406=CARTESIAN_POINT('Ctrl Pts',(1.2413030787577,3.79166666666666,2.14999999999999));
#20407=CARTESIAN_POINT('Ctrl Pts',(1.05346240894046E-14,3.84999999999999,
2.15));
#20408=CARTESIAN_POINT('Origin',(-1.80160437084306E-13,4.2,2.15));
#20409=CARTESIAN_POINT('Ctrl Pts',(0.,4.28626379701574E-17,2.5));
#20410=CARTESIAN_POINT('Ctrl Pts',(-1.44337567297406,0.0583333333333333,
2.5));
#20411=CARTESIAN_POINT('Ctrl Pts',(-2.1650635094611,0.116666666666666,1.25));
#20412=CARTESIAN_POINT('Ctrl Pts',(-2.88675134594813,0.175,1.76762539787484E-16));
#20413=CARTESIAN_POINT('Ctrl Pts',(-2.1650635094611,0.233333333333333,-1.25));
#20414=CARTESIAN_POINT('Ctrl Pts',(-1.44337567297407,0.291666666666666,
-2.5));
#20415=CARTESIAN_POINT('Ctrl Pts',(-3.06161699786838E-16,0.349999999999999,
-2.5));
#20416=CARTESIAN_POINT('Ctrl Pts',(1.44337567297406,0.408333333333333,-2.5));
#20417=CARTESIAN_POINT('Ctrl Pts',(2.1650635094611,0.466666666666666,-1.25));
#20418=CARTESIAN_POINT('Ctrl Pts',(2.88675134594813,0.524999999999999,-5.30287619362453E-16));
#20419=CARTESIAN_POINT('Ctrl Pts',(2.1650635094611,0.583333333333332,1.25));
#20420=CARTESIAN_POINT('Ctrl Pts',(1.44337567297407,0.641666666666665,2.5));
#20421=CARTESIAN_POINT('Ctrl Pts',(0.,0.699999999999999,2.5));
#20422=CARTESIAN_POINT('Ctrl Pts',(-1.44337567297406,0.758333333333332,
2.5));
#20423=CARTESIAN_POINT('Ctrl Pts',(-2.1650635094611,0.816666666666665,1.25));
#20424=CARTESIAN_POINT('Ctrl Pts',(-2.88675134594813,0.874999999999998,
1.76762539787484E-16));
#20425=CARTESIAN_POINT('Ctrl Pts',(-2.1650635094611,0.933333333333332,-1.25));
#20426=CARTESIAN_POINT('Ctrl Pts',(-1.44337567297407,0.991666666666665,
-2.5));
#20427=CARTESIAN_POINT('Ctrl Pts',(-3.06161699786838E-16,1.05,-2.5));
#20428=CARTESIAN_POINT('Ctrl Pts',(1.44337567297406,1.10833333333333,-2.5));
#20429=CARTESIAN_POINT('Ctrl Pts',(2.1650635094611,1.16666666666666,-1.25));
#20430=CARTESIAN_POINT('Ctrl Pts',(2.88675134594813,1.225,-5.30287619362453E-16));
#20431=CARTESIAN_POINT('Ctrl Pts',(2.1650635094611,1.28333333333333,1.25));
#20432=CARTESIAN_POINT('Ctrl Pts',(1.44337567297407,1.34166666666666,2.5));
#20433=CARTESIAN_POINT('Ctrl Pts',(0.,1.4,2.5));
#20434=CARTESIAN_POINT('Ctrl Pts',(-1.44337567297406,1.45833333333333,2.5));
#20435=CARTESIAN_POINT('Ctrl Pts',(-2.1650635094611,1.51666666666666,1.25));
#20436=CARTESIAN_POINT('Ctrl Pts',(-2.88675134594813,1.575,1.76762539787484E-16));
#20437=CARTESIAN_POINT('Ctrl Pts',(-2.1650635094611,1.63333333333333,-1.25));
#20438=CARTESIAN_POINT('Ctrl Pts',(-1.44337567297407,1.69166666666666,-2.5));
#20439=CARTESIAN_POINT('Ctrl Pts',(-3.06161699786838E-16,1.75,-2.5));
#20440=CARTESIAN_POINT('Ctrl Pts',(1.44337567297406,1.80833333333333,-2.5));
#20441=CARTESIAN_POINT('Ctrl Pts',(2.1650635094611,1.86666666666666,-1.25));
#20442=CARTESIAN_POINT('Ctrl Pts',(2.88675134594813,1.925,-5.30287619362453E-16));
#20443=CARTESIAN_POINT('Ctrl Pts',(2.1650635094611,1.98333333333333,1.25));
#20444=CARTESIAN_POINT('Ctrl Pts',(1.44337567297407,2.04166666666666,2.5));
#20445=CARTESIAN_POINT('Ctrl Pts',(0.,2.1,2.5));
#20446=CARTESIAN_POINT('Ctrl Pts',(-1.44337567297406,2.15833333333333,2.5));
#20447=CARTESIAN_POINT('Ctrl Pts',(-2.1650635094611,2.21666666666666,1.25));
#20448=CARTESIAN_POINT('Ctrl Pts',(-2.88675134594813,2.275,1.76762539787484E-16));
#20449=CARTESIAN_POINT('Ctrl Pts',(-2.1650635094611,2.33333333333333,-1.25));
#20450=CARTESIAN_POINT('Ctrl Pts',(-1.44337567297407,2.39166666666666,-2.5));
#20451=CARTESIAN_POINT('Ctrl Pts',(-3.06161699786838E-16,2.45,-2.5));
#20452=CARTESIAN_POINT('Ctrl Pts',(1.44337567297406,2.50833333333333,-2.5));
#20453=CARTESIAN_POINT('Ctrl Pts',(2.1650635094611,2.56666666666666,-1.25));
#20454=CARTESIAN_POINT('Ctrl Pts',(2.88675134594813,2.62499999999999,-5.30287619362453E-16));
#20455=CARTESIAN_POINT('Ctrl Pts',(2.1650635094611,2.68333333333333,1.25));
#20456=CARTESIAN_POINT('Ctrl Pts',(1.44337567297407,2.74166666666666,2.5));
#20457=CARTESIAN_POINT('Ctrl Pts',(0.,2.79999999999999,2.5));
#20458=CARTESIAN_POINT('Ctrl Pts',(-1.44337567297406,2.85833333333333,2.5));
#20459=CARTESIAN_POINT('Ctrl Pts',(-2.1650635094611,2.91666666666666,1.25));
#20460=CARTESIAN_POINT('Ctrl Pts',(-2.88675134594813,2.97499999999999,1.76762539787484E-16));
#20461=CARTESIAN_POINT('Ctrl Pts',(-2.1650635094611,3.03333333333333,-1.25));
#20462=CARTESIAN_POINT('Ctrl Pts',(-1.44337567297407,3.09166666666666,-2.5));
#20463=CARTESIAN_POINT('Ctrl Pts',(-3.06161699786838E-16,3.14999999999999,
-2.5));
#20464=CARTESIAN_POINT('Ctrl Pts',(1.44337567297406,3.20833333333333,-2.5));
#20465=CARTESIAN_POINT('Ctrl Pts',(2.1650635094611,3.26666666666666,-1.25));
#20466=CARTESIAN_POINT('Ctrl Pts',(2.88675134594813,3.32499999999999,-5.30287619362453E-16));
#20467=CARTESIAN_POINT('Ctrl Pts',(2.1650635094611,3.38333333333333,1.25));
#20468=CARTESIAN_POINT('Ctrl Pts',(1.44337567297407,3.44166666666666,2.5));
#20469=CARTESIAN_POINT('Ctrl Pts',(0.,3.49999999999999,2.5));
#20470=CARTESIAN_POINT('Ctrl Pts',(-1.44337567297406,3.55833333333333,2.5));
#20471=CARTESIAN_POINT('Ctrl Pts',(-2.1650635094611,3.61666666666666,1.25));
#20472=CARTESIAN_POINT('Ctrl Pts',(-2.88675134594813,3.67499999999999,1.76762539787484E-16));
#20473=CARTESIAN_POINT('Ctrl Pts',(-2.1650635094611,3.73333333333333,-1.25));
#20474=CARTESIAN_POINT('Ctrl Pts',(-1.44337567297407,3.79166666666666,-2.5));
#20475=CARTESIAN_POINT('Ctrl Pts',(-3.06161699786838E-16,3.84999999999999,
-2.5));
#20476=CARTESIAN_POINT('Ctrl Pts',(1.44337567297406,3.90833333333333,-2.5));
#20477=CARTESIAN_POINT('Ctrl Pts',(2.1650635094611,3.96666666666666,-1.25));
#20478=CARTESIAN_POINT('Ctrl Pts',(2.88675134594813,4.02499999999999,-5.30287619362453E-16));
#20479=CARTESIAN_POINT('Ctrl Pts',(2.1650635094611,4.08333333333333,1.25));
#20480=CARTESIAN_POINT('Ctrl Pts',(1.44337567297407,4.14166666666666,2.5));
#20481=CARTESIAN_POINT('Ctrl Pts',(0.,4.19999999999999,2.5));
#20482=CARTESIAN_POINT('Ctrl Pts',(0.,-0.205025253169417,2.5));
#20483=CARTESIAN_POINT('Ctrl Pts',(-1.44337567297406,-0.146691919836083,
2.5));
#20484=CARTESIAN_POINT('Ctrl Pts',(-2.1650635094611,-0.0883585865027503,
1.25));
#20485=CARTESIAN_POINT('Ctrl Pts',(-2.88675134594813,-0.0300252531694171,
1.76762539787484E-16));
#20486=CARTESIAN_POINT('Ctrl Pts',(-2.1650635094611,0.0283080801639162,
-1.25));
#20487=CARTESIAN_POINT('Ctrl Pts',(-1.44337567297407,0.0866414134972494,
-2.5));
#20488=CARTESIAN_POINT('Ctrl Pts',(-3.06161699786838E-16,0.144974746830583,
-2.5));
#20489=CARTESIAN_POINT('Ctrl Pts',(1.44337567297406,0.203308080163916,-2.5));
#20490=CARTESIAN_POINT('Ctrl Pts',(2.1650635094611,0.261641413497249,-1.25));
#20491=CARTESIAN_POINT('Ctrl Pts',(2.88675134594813,0.319974746830582,-5.30287619362453E-16));
#20492=CARTESIAN_POINT('Ctrl Pts',(2.1650635094611,0.378308080163915,1.25));
#20493=CARTESIAN_POINT('Ctrl Pts',(1.44337567297407,0.436641413497249,2.5));
#20494=CARTESIAN_POINT('Ctrl Pts',(0.,0.494974746830582,2.5));
#20495=CARTESIAN_POINT('Ctrl Pts',(-1.44337567297406,0.553308080163915,
2.5));
#20496=CARTESIAN_POINT('Ctrl Pts',(-2.1650635094611,0.611641413497248,1.25));
#20497=CARTESIAN_POINT('Ctrl Pts',(-2.88675134594813,0.669974746830582,
1.76762539787484E-16));
#20498=CARTESIAN_POINT('Ctrl Pts',(-2.1650635094611,0.728308080163915,-1.25));
#20499=CARTESIAN_POINT('Ctrl Pts',(-1.44337567297407,0.786641413497248,
-2.5));
#20500=CARTESIAN_POINT('Ctrl Pts',(-3.06161699786838E-16,0.844974746830581,
-2.5));
#20501=CARTESIAN_POINT('Ctrl Pts',(1.44337567297406,0.903308080163914,-2.5));
#20502=CARTESIAN_POINT('Ctrl Pts',(2.1650635094611,0.961641413497248,-1.25));
#20503=CARTESIAN_POINT('Ctrl Pts',(2.88675134594813,1.01997474683058,-5.30287619362453E-16));
#20504=CARTESIAN_POINT('Ctrl Pts',(2.1650635094611,1.07830808016391,1.25));
#20505=CARTESIAN_POINT('Ctrl Pts',(1.44337567297407,1.13664141349725,2.5));
#20506=CARTESIAN_POINT('Ctrl Pts',(0.,1.19497474683058,2.5));
#20507=CARTESIAN_POINT('Ctrl Pts',(-1.44337567297406,1.25330808016391,2.5));
#20508=CARTESIAN_POINT('Ctrl Pts',(-2.1650635094611,1.31164141349725,1.25));
#20509=CARTESIAN_POINT('Ctrl Pts',(-2.88675134594813,1.36997474683058,1.76762539787484E-16));
#20510=CARTESIAN_POINT('Ctrl Pts',(-2.1650635094611,1.42830808016391,-1.25));
#20511=CARTESIAN_POINT('Ctrl Pts',(-1.44337567297407,1.48664141349725,-2.5));
#20512=CARTESIAN_POINT('Ctrl Pts',(-3.06161699786838E-16,1.54497474683058,
-2.5));
#20513=CARTESIAN_POINT('Ctrl Pts',(1.44337567297406,1.60330808016391,-2.5));
#20514=CARTESIAN_POINT('Ctrl Pts',(2.1650635094611,1.66164141349725,-1.25));
#20515=CARTESIAN_POINT('Ctrl Pts',(2.88675134594813,1.71997474683058,-5.30287619362453E-16));
#20516=CARTESIAN_POINT('Ctrl Pts',(2.1650635094611,1.77830808016391,1.25));
#20517=CARTESIAN_POINT('Ctrl Pts',(1.44337567297407,1.83664141349725,2.5));
#20518=CARTESIAN_POINT('Ctrl Pts',(0.,1.89497474683058,2.5));
#20519=CARTESIAN_POINT('Ctrl Pts',(-1.44337567297406,1.95330808016391,2.5));
#20520=CARTESIAN_POINT('Ctrl Pts',(-2.1650635094611,2.01164141349725,1.25));
#20521=CARTESIAN_POINT('Ctrl Pts',(-2.88675134594813,2.06997474683058,1.76762539787484E-16));
#20522=CARTESIAN_POINT('Ctrl Pts',(-2.1650635094611,2.12830808016391,-1.25));
#20523=CARTESIAN_POINT('Ctrl Pts',(-1.44337567297407,2.18664141349725,-2.5));
#20524=CARTESIAN_POINT('Ctrl Pts',(-3.06161699786838E-16,2.24497474683058,
-2.5));
#20525=CARTESIAN_POINT('Ctrl Pts',(1.44337567297406,2.30330808016391,-2.5));
#20526=CARTESIAN_POINT('Ctrl Pts',(2.1650635094611,2.36164141349724,-1.25));
#20527=CARTESIAN_POINT('Ctrl Pts',(2.88675134594813,2.41997474683058,-5.30287619362453E-16));
#20528=CARTESIAN_POINT('Ctrl Pts',(2.1650635094611,2.47830808016391,1.25));
#20529=CARTESIAN_POINT('Ctrl Pts',(1.44337567297407,2.53664141349724,2.5));
#20530=CARTESIAN_POINT('Ctrl Pts',(0.,2.59497474683058,2.5));
#20531=CARTESIAN_POINT('Ctrl Pts',(-1.44337567297406,2.65330808016391,2.5));
#20532=CARTESIAN_POINT('Ctrl Pts',(-2.1650635094611,2.71164141349724,1.25));
#20533=CARTESIAN_POINT('Ctrl Pts',(-2.88675134594813,2.76997474683058,1.76762539787484E-16));
#20534=CARTESIAN_POINT('Ctrl Pts',(-2.1650635094611,2.82830808016391,-1.25));
#20535=CARTESIAN_POINT('Ctrl Pts',(-1.44337567297407,2.88664141349724,-2.5));
#20536=CARTESIAN_POINT('Ctrl Pts',(-3.06161699786838E-16,2.94497474683058,
-2.5));
#20537=CARTESIAN_POINT('Ctrl Pts',(1.44337567297406,3.00330808016391,-2.5));
#20538=CARTESIAN_POINT('Ctrl Pts',(2.1650635094611,3.06164141349724,-1.25));
#20539=CARTESIAN_POINT('Ctrl Pts',(2.88675134594813,3.11997474683058,-5.30287619362453E-16));
#20540=CARTESIAN_POINT('Ctrl Pts',(2.1650635094611,3.17830808016391,1.25));
#20541=CARTESIAN_POINT('Ctrl Pts',(1.44337567297407,3.23664141349724,2.5));
#20542=CARTESIAN_POINT('Ctrl Pts',(0.,3.29497474683058,2.5));
#20543=CARTESIAN_POINT('Ctrl Pts',(-1.44337567297406,3.35330808016391,2.5));
#20544=CARTESIAN_POINT('Ctrl Pts',(-2.1650635094611,3.41164141349724,1.25));
#20545=CARTESIAN_POINT('Ctrl Pts',(-2.88675134594813,3.46997474683058,1.76762539787484E-16));
#20546=CARTESIAN_POINT('Ctrl Pts',(-2.1650635094611,3.52830808016391,-1.25));
#20547=CARTESIAN_POINT('Ctrl Pts',(-1.44337567297407,3.58664141349724,-2.5));
#20548=CARTESIAN_POINT('Ctrl Pts',(-3.06161699786838E-16,3.64497474683058,
-2.5));
#20549=CARTESIAN_POINT('Ctrl Pts',(1.44337567297406,3.70330808016391,-2.5));
#20550=CARTESIAN_POINT('Ctrl Pts',(2.1650635094611,3.76164141349724,-1.25));
#20551=CARTESIAN_POINT('Ctrl Pts',(2.88675134594813,3.81997474683058,-5.30287619362453E-16));
#20552=CARTESIAN_POINT('Ctrl Pts',(2.1650635094611,3.87830808016391,1.25));
#20553=CARTESIAN_POINT('Ctrl Pts',(1.44337567297407,3.93664141349724,2.5));
#20554=CARTESIAN_POINT('Ctrl Pts',(0.,3.99497474683058,2.5));
#20555=CARTESIAN_POINT('Ctrl Pts',(0.,-0.35,2.35502525316942));
#20556=CARTESIAN_POINT('Ctrl Pts',(-1.35967446386573,-0.291666666666667,
2.35502525316942));
#20557=CARTESIAN_POINT('Ctrl Pts',(-2.03951169579859,-0.233333333333334,
1.17751262658471));
#20558=CARTESIAN_POINT('Ctrl Pts',(-2.71934892773146,-0.175,1.66512098005556E-16));
#20559=CARTESIAN_POINT('Ctrl Pts',(-2.03951169579859,-0.116666666666667,
-1.17751262658471));
#20560=CARTESIAN_POINT('Ctrl Pts',(-1.35967446386573,-0.0583333333333339,
-2.35502525316942));
#20561=CARTESIAN_POINT('Ctrl Pts',(-2.88407413820511E-16,-7.04731412115578E-16,
-2.35502525316942));
#20562=CARTESIAN_POINT('Ctrl Pts',(1.35967446386573,0.0583333333333326,
-2.35502525316942));
#20563=CARTESIAN_POINT('Ctrl Pts',(2.03951169579859,0.116666666666666,-1.17751262658471));
#20564=CARTESIAN_POINT('Ctrl Pts',(2.71934892773146,0.174999999999999,-4.99536294016668E-16));
#20565=CARTESIAN_POINT('Ctrl Pts',(2.03951169579859,0.233333333333332,1.17751262658471));
#20566=CARTESIAN_POINT('Ctrl Pts',(1.35967446386573,0.291666666666665,2.35502525316942));
#20567=CARTESIAN_POINT('Ctrl Pts',(0.,0.349999999999999,2.35502525316942));
#20568=CARTESIAN_POINT('Ctrl Pts',(-1.35967446386573,0.408333333333332,
2.35502525316942));
#20569=CARTESIAN_POINT('Ctrl Pts',(-2.03951169579859,0.466666666666665,
1.17751262658471));
#20570=CARTESIAN_POINT('Ctrl Pts',(-2.71934892773146,0.524999999999998,
1.66512098005556E-16));
#20571=CARTESIAN_POINT('Ctrl Pts',(-2.03951169579859,0.583333333333332,
-1.17751262658471));
#20572=CARTESIAN_POINT('Ctrl Pts',(-1.35967446386573,0.641666666666665,
-2.35502525316942));
#20573=CARTESIAN_POINT('Ctrl Pts',(-2.88407413820511E-16,0.699999999999998,
-2.35502525316942));
#20574=CARTESIAN_POINT('Ctrl Pts',(1.35967446386573,0.758333333333331,-2.35502525316942));
#20575=CARTESIAN_POINT('Ctrl Pts',(2.03951169579859,0.816666666666664,-1.17751262658471));
#20576=CARTESIAN_POINT('Ctrl Pts',(2.71934892773146,0.874999999999998,-4.99536294016668E-16));
#20577=CARTESIAN_POINT('Ctrl Pts',(2.03951169579859,0.933333333333331,1.17751262658471));
#20578=CARTESIAN_POINT('Ctrl Pts',(1.35967446386573,0.991666666666664,2.35502525316942));
#20579=CARTESIAN_POINT('Ctrl Pts',(0.,1.05,2.35502525316942));
#20580=CARTESIAN_POINT('Ctrl Pts',(-1.35967446386573,1.10833333333333,2.35502525316942));
#20581=CARTESIAN_POINT('Ctrl Pts',(-2.03951169579859,1.16666666666666,1.17751262658471));
#20582=CARTESIAN_POINT('Ctrl Pts',(-2.71934892773146,1.225,1.66512098005556E-16));
#20583=CARTESIAN_POINT('Ctrl Pts',(-2.03951169579859,1.28333333333333,-1.17751262658471));
#20584=CARTESIAN_POINT('Ctrl Pts',(-1.35967446386573,1.34166666666666,-2.35502525316942));
#20585=CARTESIAN_POINT('Ctrl Pts',(-2.88407413820511E-16,1.4,-2.35502525316942));
#20586=CARTESIAN_POINT('Ctrl Pts',(1.35967446386573,1.45833333333333,-2.35502525316942));
#20587=CARTESIAN_POINT('Ctrl Pts',(2.03951169579859,1.51666666666666,-1.17751262658471));
#20588=CARTESIAN_POINT('Ctrl Pts',(2.71934892773146,1.575,-4.99536294016668E-16));
#20589=CARTESIAN_POINT('Ctrl Pts',(2.03951169579859,1.63333333333333,1.17751262658471));
#20590=CARTESIAN_POINT('Ctrl Pts',(1.35967446386573,1.69166666666666,2.35502525316942));
#20591=CARTESIAN_POINT('Ctrl Pts',(0.,1.75,2.35502525316942));
#20592=CARTESIAN_POINT('Ctrl Pts',(-1.35967446386573,1.80833333333333,2.35502525316942));
#20593=CARTESIAN_POINT('Ctrl Pts',(-2.03951169579859,1.86666666666666,1.17751262658471));
#20594=CARTESIAN_POINT('Ctrl Pts',(-2.71934892773146,1.925,1.66512098005556E-16));
#20595=CARTESIAN_POINT('Ctrl Pts',(-2.03951169579859,1.98333333333333,-1.17751262658471));
#20596=CARTESIAN_POINT('Ctrl Pts',(-1.35967446386573,2.04166666666666,-2.35502525316942));
#20597=CARTESIAN_POINT('Ctrl Pts',(-2.88407413820511E-16,2.09999999999999,
-2.35502525316942));
#20598=CARTESIAN_POINT('Ctrl Pts',(1.35967446386573,2.15833333333333,-2.35502525316942));
#20599=CARTESIAN_POINT('Ctrl Pts',(2.03951169579859,2.21666666666666,-1.17751262658471));
#20600=CARTESIAN_POINT('Ctrl Pts',(2.71934892773146,2.275,-4.99536294016668E-16));
#20601=CARTESIAN_POINT('Ctrl Pts',(2.03951169579859,2.33333333333333,1.17751262658471));
#20602=CARTESIAN_POINT('Ctrl Pts',(1.35967446386573,2.39166666666666,2.35502525316942));
#20603=CARTESIAN_POINT('Ctrl Pts',(0.,2.44999999999999,2.35502525316942));
#20604=CARTESIAN_POINT('Ctrl Pts',(-1.35967446386573,2.50833333333333,2.35502525316942));
#20605=CARTESIAN_POINT('Ctrl Pts',(-2.03951169579859,2.56666666666666,1.17751262658471));
#20606=CARTESIAN_POINT('Ctrl Pts',(-2.71934892773146,2.62499999999999,1.66512098005556E-16));
#20607=CARTESIAN_POINT('Ctrl Pts',(-2.03951169579859,2.68333333333333,-1.17751262658471));
#20608=CARTESIAN_POINT('Ctrl Pts',(-1.35967446386573,2.74166666666666,-2.35502525316942));
#20609=CARTESIAN_POINT('Ctrl Pts',(-2.88407413820511E-16,2.79999999999999,
-2.35502525316942));
#20610=CARTESIAN_POINT('Ctrl Pts',(1.35967446386573,2.85833333333333,-2.35502525316942));
#20611=CARTESIAN_POINT('Ctrl Pts',(2.03951169579859,2.91666666666666,-1.17751262658471));
#20612=CARTESIAN_POINT('Ctrl Pts',(2.71934892773146,2.97499999999999,-4.99536294016668E-16));
#20613=CARTESIAN_POINT('Ctrl Pts',(2.03951169579859,3.03333333333333,1.17751262658471));
#20614=CARTESIAN_POINT('Ctrl Pts',(1.35967446386573,3.09166666666666,2.35502525316942));
#20615=CARTESIAN_POINT('Ctrl Pts',(0.,3.14999999999999,2.35502525316942));
#20616=CARTESIAN_POINT('Ctrl Pts',(-1.35967446386573,3.20833333333333,2.35502525316942));
#20617=CARTESIAN_POINT('Ctrl Pts',(-2.03951169579859,3.26666666666666,1.17751262658471));
#20618=CARTESIAN_POINT('Ctrl Pts',(-2.71934892773146,3.32499999999999,1.66512098005556E-16));
#20619=CARTESIAN_POINT('Ctrl Pts',(-2.03951169579859,3.38333333333333,-1.17751262658471));
#20620=CARTESIAN_POINT('Ctrl Pts',(-1.35967446386573,3.44166666666666,-2.35502525316942));
#20621=CARTESIAN_POINT('Ctrl Pts',(-2.88407413820511E-16,3.49999999999999,
-2.35502525316942));
#20622=CARTESIAN_POINT('Ctrl Pts',(1.35967446386573,3.55833333333333,-2.35502525316942));
#20623=CARTESIAN_POINT('Ctrl Pts',(2.03951169579859,3.61666666666666,-1.17751262658471));
#20624=CARTESIAN_POINT('Ctrl Pts',(2.71934892773146,3.67499999999999,-4.99536294016668E-16));
#20625=CARTESIAN_POINT('Ctrl Pts',(2.03951169579859,3.73333333333332,1.17751262658471));
#20626=CARTESIAN_POINT('Ctrl Pts',(1.35967446386573,3.79166666666666,2.35502525316942));
#20627=CARTESIAN_POINT('Ctrl Pts',(0.,3.84999999999999,2.35502525316942));
#20628=CARTESIAN_POINT('Ctrl Pts',(0.,-0.35,2.15));
#20629=CARTESIAN_POINT('Ctrl Pts',(-1.2413030787577,-0.291666666666667,
2.15));
#20630=CARTESIAN_POINT('Ctrl Pts',(-1.86195461813654,-0.233333333333334,
1.075));
#20631=CARTESIAN_POINT('Ctrl Pts',(-2.48260615751539,-0.175,1.52015784217237E-16));
#20632=CARTESIAN_POINT('Ctrl Pts',(-1.86195461813654,-0.116666666666667,
-1.075));
#20633=CARTESIAN_POINT('Ctrl Pts',(-1.2413030787577,-0.058333333333334,
-2.15));
#20634=CARTESIAN_POINT('Ctrl Pts',(-2.63299061816681E-16,-7.58941520739853E-16,
-2.15));
#20635=CARTESIAN_POINT('Ctrl Pts',(1.24130307875769,0.0583333333333325,
-2.15));
#20636=CARTESIAN_POINT('Ctrl Pts',(1.86195461813654,0.116666666666666,-1.075));
#20637=CARTESIAN_POINT('Ctrl Pts',(2.48260615751539,0.174999999999999,-4.5604735265171E-16));
#20638=CARTESIAN_POINT('Ctrl Pts',(1.86195461813654,0.233333333333332,1.075));
#20639=CARTESIAN_POINT('Ctrl Pts',(1.2413030787577,0.291666666666665,2.15));
#20640=CARTESIAN_POINT('Ctrl Pts',(0.,0.349999999999999,2.15));
#20641=CARTESIAN_POINT('Ctrl Pts',(-1.2413030787577,0.408333333333332,2.15));
#20642=CARTESIAN_POINT('Ctrl Pts',(-1.86195461813654,0.466666666666665,
1.075));
#20643=CARTESIAN_POINT('Ctrl Pts',(-2.48260615751539,0.524999999999998,
1.52015784217237E-16));
#20644=CARTESIAN_POINT('Ctrl Pts',(-1.86195461813654,0.583333333333331,
-1.075));
#20645=CARTESIAN_POINT('Ctrl Pts',(-1.2413030787577,0.641666666666665,-2.15));
#20646=CARTESIAN_POINT('Ctrl Pts',(-2.63299061816681E-16,0.699999999999998,
-2.15));
#20647=CARTESIAN_POINT('Ctrl Pts',(1.24130307875769,0.758333333333331,-2.15));
#20648=CARTESIAN_POINT('Ctrl Pts',(1.86195461813654,0.816666666666664,-1.075));
#20649=CARTESIAN_POINT('Ctrl Pts',(2.48260615751539,0.874999999999997,-4.5604735265171E-16));
#20650=CARTESIAN_POINT('Ctrl Pts',(1.86195461813654,0.933333333333331,1.075));
#20651=CARTESIAN_POINT('Ctrl Pts',(1.2413030787577,0.991666666666664,2.15));
#20652=CARTESIAN_POINT('Ctrl Pts',(0.,1.05,2.15));
#20653=CARTESIAN_POINT('Ctrl Pts',(-1.2413030787577,1.10833333333333,2.15));
#20654=CARTESIAN_POINT('Ctrl Pts',(-1.86195461813654,1.16666666666666,1.075));
#20655=CARTESIAN_POINT('Ctrl Pts',(-2.48260615751539,1.225,1.52015784217237E-16));
#20656=CARTESIAN_POINT('Ctrl Pts',(-1.86195461813654,1.28333333333333,-1.075));
#20657=CARTESIAN_POINT('Ctrl Pts',(-1.2413030787577,1.34166666666666,-2.15));
#20658=CARTESIAN_POINT('Ctrl Pts',(-2.63299061816681E-16,1.4,-2.15));
#20659=CARTESIAN_POINT('Ctrl Pts',(1.24130307875769,1.45833333333333,-2.15));
#20660=CARTESIAN_POINT('Ctrl Pts',(1.86195461813654,1.51666666666666,-1.075));
#20661=CARTESIAN_POINT('Ctrl Pts',(2.48260615751539,1.575,-4.5604735265171E-16));
#20662=CARTESIAN_POINT('Ctrl Pts',(1.86195461813654,1.63333333333333,1.075));
#20663=CARTESIAN_POINT('Ctrl Pts',(1.2413030787577,1.69166666666666,2.15));
#20664=CARTESIAN_POINT('Ctrl Pts',(0.,1.75,2.15));
#20665=CARTESIAN_POINT('Ctrl Pts',(-1.2413030787577,1.80833333333333,2.15));
#20666=CARTESIAN_POINT('Ctrl Pts',(-1.86195461813654,1.86666666666666,1.075));
#20667=CARTESIAN_POINT('Ctrl Pts',(-2.48260615751539,1.925,1.52015784217237E-16));
#20668=CARTESIAN_POINT('Ctrl Pts',(-1.86195461813654,1.98333333333333,-1.075));
#20669=CARTESIAN_POINT('Ctrl Pts',(-1.2413030787577,2.04166666666666,-2.15));
#20670=CARTESIAN_POINT('Ctrl Pts',(-2.63299061816681E-16,2.1,-2.15));
#20671=CARTESIAN_POINT('Ctrl Pts',(1.24130307875769,2.15833333333333,-2.15));
#20672=CARTESIAN_POINT('Ctrl Pts',(1.86195461813654,2.21666666666666,-1.075));
#20673=CARTESIAN_POINT('Ctrl Pts',(2.48260615751539,2.275,-4.5604735265171E-16));
#20674=CARTESIAN_POINT('Ctrl Pts',(1.86195461813654,2.33333333333333,1.075));
#20675=CARTESIAN_POINT('Ctrl Pts',(1.2413030787577,2.39166666666666,2.15));
#20676=CARTESIAN_POINT('Ctrl Pts',(0.,2.44999999999999,2.15));
#20677=CARTESIAN_POINT('Ctrl Pts',(-1.2413030787577,2.50833333333333,2.15));
#20678=CARTESIAN_POINT('Ctrl Pts',(-1.86195461813654,2.56666666666666,1.075));
#20679=CARTESIAN_POINT('Ctrl Pts',(-2.48260615751539,2.62499999999999,1.52015784217237E-16));
#20680=CARTESIAN_POINT('Ctrl Pts',(-1.86195461813654,2.68333333333333,-1.075));
#20681=CARTESIAN_POINT('Ctrl Pts',(-1.2413030787577,2.74166666666666,-2.15));
#20682=CARTESIAN_POINT('Ctrl Pts',(-2.63299061816681E-16,2.79999999999999,
-2.15));
#20683=CARTESIAN_POINT('Ctrl Pts',(1.24130307875769,2.85833333333333,-2.15));
#20684=CARTESIAN_POINT('Ctrl Pts',(1.86195461813654,2.91666666666666,-1.075));
#20685=CARTESIAN_POINT('Ctrl Pts',(2.48260615751539,2.97499999999999,-4.5604735265171E-16));
#20686=CARTESIAN_POINT('Ctrl Pts',(1.86195461813654,3.03333333333333,1.075));
#20687=CARTESIAN_POINT('Ctrl Pts',(1.2413030787577,3.09166666666666,2.15));
#20688=CARTESIAN_POINT('Ctrl Pts',(0.,3.14999999999999,2.15));
#20689=CARTESIAN_POINT('Ctrl Pts',(-1.2413030787577,3.20833333333333,2.15));
#20690=CARTESIAN_POINT('Ctrl Pts',(-1.86195461813654,3.26666666666666,1.075));
#20691=CARTESIAN_POINT('Ctrl Pts',(-2.48260615751539,3.32499999999999,1.52015784217237E-16));
#20692=CARTESIAN_POINT('Ctrl Pts',(-1.86195461813654,3.38333333333333,-1.075));
#20693=CARTESIAN_POINT('Ctrl Pts',(-1.2413030787577,3.44166666666666,-2.15));
#20694=CARTESIAN_POINT('Ctrl Pts',(-2.63299061816681E-16,3.49999999999999,
-2.15));
#20695=CARTESIAN_POINT('Ctrl Pts',(1.24130307875769,3.55833333333333,-2.15));
#20696=CARTESIAN_POINT('Ctrl Pts',(1.86195461813654,3.61666666666666,-1.075));
#20697=CARTESIAN_POINT('Ctrl Pts',(2.48260615751539,3.67499999999999,-4.5604735265171E-16));
#20698=CARTESIAN_POINT('Ctrl Pts',(1.86195461813654,3.73333333333333,1.075));
#20699=CARTESIAN_POINT('Ctrl Pts',(1.2413030787577,3.79166666666666,2.15));
#20700=CARTESIAN_POINT('Ctrl Pts',(0.,3.84999999999999,2.15));
#20701=CARTESIAN_POINT('',(0.,4.28626379701574E-17,2.5));
#20702=CARTESIAN_POINT('Origin',(0.,0.,2.15));
#20703=CARTESIAN_POINT('',(-1.02907469966573E-13,4.2,2.5));
#20704=CARTESIAN_POINT('Ctrl Pts',(0.,4.28626379701574E-17,2.5));
#20705=CARTESIAN_POINT('Ctrl Pts',(-1.44337567297406,0.0583333333333333,
2.5));
#20706=CARTESIAN_POINT('Ctrl Pts',(-2.1650635094611,0.116666666666666,1.25));
#20707=CARTESIAN_POINT('Ctrl Pts',(-2.88675134594813,0.175,1.76762539787484E-16));
#20708=CARTESIAN_POINT('Ctrl Pts',(-2.1650635094611,0.233333333333333,-1.25));
#20709=CARTESIAN_POINT('Ctrl Pts',(-1.44337567297407,0.291666666666666,
-2.5));
#20710=CARTESIAN_POINT('Ctrl Pts',(-3.06161699786838E-16,0.349999999999999,
-2.5));
#20711=CARTESIAN_POINT('Ctrl Pts',(1.44337567297406,0.408333333333333,-2.5));
#20712=CARTESIAN_POINT('Ctrl Pts',(2.1650635094611,0.466666666666666,-1.25));
#20713=CARTESIAN_POINT('Ctrl Pts',(2.88675134594813,0.524999999999999,-5.30287619362453E-16));
#20714=CARTESIAN_POINT('Ctrl Pts',(2.1650635094611,0.583333333333332,1.25));
#20715=CARTESIAN_POINT('Ctrl Pts',(1.44337567297407,0.641666666666665,2.5));
#20716=CARTESIAN_POINT('Ctrl Pts',(6.12323399573677E-16,0.699999999999999,
2.5));
#20717=CARTESIAN_POINT('Ctrl Pts',(-1.44337567297406,0.758333333333332,
2.5));
#20718=CARTESIAN_POINT('Ctrl Pts',(-2.1650635094611,0.816666666666665,1.25));
#20719=CARTESIAN_POINT('Ctrl Pts',(-2.88675134594813,0.874999999999998,
3.44776294744884E-15));
#20720=CARTESIAN_POINT('Ctrl Pts',(-2.1650635094611,0.933333333333332,-1.25));
#20721=CARTESIAN_POINT('Ctrl Pts',(-1.44337567297407,0.991666666666665,
-2.5));
#20722=CARTESIAN_POINT('Ctrl Pts',(-9.18485099360515E-16,1.05,-2.5));
#20723=CARTESIAN_POINT('Ctrl Pts',(1.44337567297406,1.10833333333333,-2.5));
#20724=CARTESIAN_POINT('Ctrl Pts',(2.16506350946109,1.16666666666666,-1.25));
#20725=CARTESIAN_POINT('Ctrl Pts',(2.88675134594813,1.225,-1.23733777851239E-15));
#20726=CARTESIAN_POINT('Ctrl Pts',(2.1650635094611,1.28333333333333,1.25));
#20727=CARTESIAN_POINT('Ctrl Pts',(1.44337567297407,1.34166666666666,2.5));
#20728=CARTESIAN_POINT('Ctrl Pts',(1.22464679914735E-15,1.4,2.5));
#20729=CARTESIAN_POINT('Ctrl Pts',(-1.44337567297406,1.45833333333333,2.5));
#20730=CARTESIAN_POINT('Ctrl Pts',(-2.16506350946109,1.51666666666666,1.25));
#20731=CARTESIAN_POINT('Ctrl Pts',(-2.88675134594813,1.575,6.7187633551102E-15));
#20732=CARTESIAN_POINT('Ctrl Pts',(-2.1650635094611,1.63333333333333,-1.25));
#20733=CARTESIAN_POINT('Ctrl Pts',(-1.44337567297407,1.69166666666666,-2.5));
#20734=CARTESIAN_POINT('Ctrl Pts',(-5.97170059743482E-15,1.75,-2.5));
#20735=CARTESIAN_POINT('Ctrl Pts',(1.44337567297406,1.80833333333333,-2.5));
#20736=CARTESIAN_POINT('Ctrl Pts',(2.16506350946109,1.86666666666666,-1.25));
#20737=CARTESIAN_POINT('Ctrl Pts',(2.88675134594813,1.925,-7.07228843468517E-15));
#20738=CARTESIAN_POINT('Ctrl Pts',(2.1650635094611,1.98333333333333,1.24999999999999));
#20739=CARTESIAN_POINT('Ctrl Pts',(1.44337567297407,2.04166666666666,2.49999999999999));
#20740=CARTESIAN_POINT('Ctrl Pts',(1.83697019872103E-15,2.1,2.5));
#20741=CARTESIAN_POINT('Ctrl Pts',(-1.44337567297406,2.15833333333333,2.5));
#20742=CARTESIAN_POINT('Ctrl Pts',(-2.16506350946109,2.21666666666666,1.25));
#20743=CARTESIAN_POINT('Ctrl Pts',(-2.88675134594813,2.275,7.42581351426014E-15));
#20744=CARTESIAN_POINT('Ctrl Pts',(-2.1650635094611,2.33333333333333,-1.24999999999999));
#20745=CARTESIAN_POINT('Ctrl Pts',(-1.44337567297407,2.39166666666666,-2.49999999999999));
#20746=CARTESIAN_POINT('Ctrl Pts',(-2.14313189850787E-15,2.45,-2.5));
#20747=CARTESIAN_POINT('Ctrl Pts',(1.44337567297406,2.50833333333333,-2.5));
#20748=CARTESIAN_POINT('Ctrl Pts',(2.16506350946109,2.56666666666666,-1.25));
#20749=CARTESIAN_POINT('Ctrl Pts',(2.88675134594813,2.625,-7.7793385938351E-15));
#20750=CARTESIAN_POINT('Ctrl Pts',(2.1650635094611,2.68333333333333,1.24999999999999));
#20751=CARTESIAN_POINT('Ctrl Pts',(1.44337567297407,2.74166666666666,2.49999999999999));
#20752=CARTESIAN_POINT('Ctrl Pts',(2.44929359829471E-15,2.79999999999999,
2.5));
#20753=CARTESIAN_POINT('Ctrl Pts',(-1.44337567297406,2.85833333333333,2.5));
#20754=CARTESIAN_POINT('Ctrl Pts',(-2.16506350946109,2.91666666666666,1.25));
#20755=CARTESIAN_POINT('Ctrl Pts',(-2.88675134594813,2.97499999999999,8.13286367341007E-15));
#20756=CARTESIAN_POINT('Ctrl Pts',(-2.1650635094611,3.03333333333333,-1.24999999999999));
#20757=CARTESIAN_POINT('Ctrl Pts',(-1.44337567297407,3.09166666666666,-2.49999999999999));
#20758=CARTESIAN_POINT('Ctrl Pts',(-1.16372394950828E-14,3.14999999999999,
-2.5));
#20759=CARTESIAN_POINT('Ctrl Pts',(1.44337567297406,3.20833333333333,-2.5));
#20760=CARTESIAN_POINT('Ctrl Pts',(2.16506350946109,3.26666666666666,-1.25000000000001));
#20761=CARTESIAN_POINT('Ctrl Pts',(2.88675134594813,3.32499999999999,-8.48638875298504E-15));
#20762=CARTESIAN_POINT('Ctrl Pts',(2.1650635094611,3.38333333333333,1.24999999999999));
#20763=CARTESIAN_POINT('Ctrl Pts',(1.44337567297407,3.44166666666666,2.49999999999999));
#20764=CARTESIAN_POINT('Ctrl Pts',(1.19434011948696E-14,3.49999999999999,
2.5));
#20765=CARTESIAN_POINT('Ctrl Pts',(-1.44337567297406,3.55833333333333,2.5));
#20766=CARTESIAN_POINT('Ctrl Pts',(-2.16506350946109,3.61666666666666,1.25000000000001));
#20767=CARTESIAN_POINT('Ctrl Pts',(-2.88675134594813,3.67499999999999,1.90957148266057E-14));
#20768=CARTESIAN_POINT('Ctrl Pts',(-2.1650635094611,3.73333333333333,-1.24999999999999));
#20769=CARTESIAN_POINT('Ctrl Pts',(-1.44337567297407,3.79166666666666,-2.5));
#20770=CARTESIAN_POINT('Ctrl Pts',(-1.22495628946565E-14,3.84999999999999,
-2.5));
#20771=CARTESIAN_POINT('Ctrl Pts',(1.44337567297406,3.90833333333333,-2.5));
#20772=CARTESIAN_POINT('Ctrl Pts',(2.16506350946109,3.96666666666666,-1.25000000000001));
#20773=CARTESIAN_POINT('Ctrl Pts',(2.88675134594813,4.02499999999999,-9.19343891213498E-15));
#20774=CARTESIAN_POINT('Ctrl Pts',(2.16506350946111,4.08333333333333,1.24999999999998));
#20775=CARTESIAN_POINT('Ctrl Pts',(1.44337567297408,4.14166666666666,2.49999999999999));
#20776=CARTESIAN_POINT('Ctrl Pts',(-1.02907469966573E-13,4.2,2.5));
#20777=CARTESIAN_POINT('Origin',(-1.80160437084306E-13,4.2,2.15));
#20778=CARTESIAN_POINT('Ctrl Pts',(0.,0.35,2.15));
#20779=CARTESIAN_POINT('Ctrl Pts',(-1.2413030787577,0.408333333333333,2.15));
#20780=CARTESIAN_POINT('Ctrl Pts',(-1.86195461813654,0.466666666666667,
1.075));
#20781=CARTESIAN_POINT('Ctrl Pts',(-2.48260615751539,0.525,1.52015784217237E-16));
#20782=CARTESIAN_POINT('Ctrl Pts',(-1.86195461813654,0.583333333333333,
-1.075));
#20783=CARTESIAN_POINT('Ctrl Pts',(-1.2413030787577,0.641666666666666,-2.15));
#20784=CARTESIAN_POINT('Ctrl Pts',(-2.63299061816681E-16,0.699999999999999,
-2.15));
#20785=CARTESIAN_POINT('Ctrl Pts',(1.24130307875769,0.758333333333333,-2.15));
#20786=CARTESIAN_POINT('Ctrl Pts',(1.86195461813654,0.816666666666666,-1.075));
#20787=CARTESIAN_POINT('Ctrl Pts',(2.48260615751539,0.874999999999999,-4.5604735265171E-16));
#20788=CARTESIAN_POINT('Ctrl Pts',(1.86195461813654,0.933333333333332,1.075));
#20789=CARTESIAN_POINT('Ctrl Pts',(1.2413030787577,0.991666666666666,2.15));
#20790=CARTESIAN_POINT('Ctrl Pts',(0.,1.05,2.15));
#20791=CARTESIAN_POINT('Ctrl Pts',(-1.2413030787577,1.10833333333333,2.15));
#20792=CARTESIAN_POINT('Ctrl Pts',(-1.86195461813654,1.16666666666667,1.075));
#20793=CARTESIAN_POINT('Ctrl Pts',(-2.48260615751539,1.225,1.52015784217237E-16));
#20794=CARTESIAN_POINT('Ctrl Pts',(-1.86195461813654,1.28333333333333,-1.075));
#20795=CARTESIAN_POINT('Ctrl Pts',(-1.2413030787577,1.34166666666666,-2.15));
#20796=CARTESIAN_POINT('Ctrl Pts',(-2.63299061816681E-16,1.4,-2.15));
#20797=CARTESIAN_POINT('Ctrl Pts',(1.24130307875769,1.45833333333333,-2.15));
#20798=CARTESIAN_POINT('Ctrl Pts',(1.86195461813654,1.51666666666666,-1.075));
#20799=CARTESIAN_POINT('Ctrl Pts',(2.48260615751539,1.575,-4.5604735265171E-16));
#20800=CARTESIAN_POINT('Ctrl Pts',(1.86195461813654,1.63333333333333,1.075));
#20801=CARTESIAN_POINT('Ctrl Pts',(1.2413030787577,1.69166666666666,2.15));
#20802=CARTESIAN_POINT('Ctrl Pts',(0.,1.75,2.15));
#20803=CARTESIAN_POINT('Ctrl Pts',(-1.2413030787577,1.80833333333333,2.15));
#20804=CARTESIAN_POINT('Ctrl Pts',(-1.86195461813654,1.86666666666666,1.075));
#20805=CARTESIAN_POINT('Ctrl Pts',(-2.48260615751539,1.925,1.52015784217237E-16));
#20806=CARTESIAN_POINT('Ctrl Pts',(-1.86195461813654,1.98333333333333,-1.075));
#20807=CARTESIAN_POINT('Ctrl Pts',(-1.2413030787577,2.04166666666666,-2.15));
#20808=CARTESIAN_POINT('Ctrl Pts',(-2.63299061816681E-16,2.1,-2.15));
#20809=CARTESIAN_POINT('Ctrl Pts',(1.24130307875769,2.15833333333333,-2.15));
#20810=CARTESIAN_POINT('Ctrl Pts',(1.86195461813654,2.21666666666666,-1.075));
#20811=CARTESIAN_POINT('Ctrl Pts',(2.48260615751539,2.275,-4.5604735265171E-16));
#20812=CARTESIAN_POINT('Ctrl Pts',(1.86195461813654,2.33333333333333,1.075));
#20813=CARTESIAN_POINT('Ctrl Pts',(1.2413030787577,2.39166666666666,2.15));
#20814=CARTESIAN_POINT('Ctrl Pts',(0.,2.45,2.15));
#20815=CARTESIAN_POINT('Ctrl Pts',(-1.2413030787577,2.50833333333333,2.15));
#20816=CARTESIAN_POINT('Ctrl Pts',(-1.86195461813654,2.56666666666666,1.075));
#20817=CARTESIAN_POINT('Ctrl Pts',(-2.48260615751539,2.625,1.52015784217237E-16));
#20818=CARTESIAN_POINT('Ctrl Pts',(-1.86195461813654,2.68333333333333,-1.075));
#20819=CARTESIAN_POINT('Ctrl Pts',(-1.2413030787577,2.74166666666666,-2.15));
#20820=CARTESIAN_POINT('Ctrl Pts',(-2.63299061816681E-16,2.8,-2.15));
#20821=CARTESIAN_POINT('Ctrl Pts',(1.24130307875769,2.85833333333333,-2.15));
#20822=CARTESIAN_POINT('Ctrl Pts',(1.86195461813654,2.91666666666666,-1.075));
#20823=CARTESIAN_POINT('Ctrl Pts',(2.48260615751539,2.97499999999999,-4.5604735265171E-16));
#20824=CARTESIAN_POINT('Ctrl Pts',(1.86195461813654,3.03333333333333,1.075));
#20825=CARTESIAN_POINT('Ctrl Pts',(1.2413030787577,3.09166666666666,2.15));
#20826=CARTESIAN_POINT('Ctrl Pts',(0.,3.15,2.15));
#20827=CARTESIAN_POINT('Ctrl Pts',(-1.2413030787577,3.20833333333333,2.15));
#20828=CARTESIAN_POINT('Ctrl Pts',(-1.86195461813654,3.26666666666666,1.075));
#20829=CARTESIAN_POINT('Ctrl Pts',(-2.48260615751539,3.32499999999999,1.52015784217237E-16));
#20830=CARTESIAN_POINT('Ctrl Pts',(-1.86195461813654,3.38333333333333,-1.075));
#20831=CARTESIAN_POINT('Ctrl Pts',(-1.2413030787577,3.44166666666666,-2.15));
#20832=CARTESIAN_POINT('Ctrl Pts',(-2.63299061816681E-16,3.49999999999999,
-2.15));
#20833=CARTESIAN_POINT('Ctrl Pts',(1.24130307875769,3.55833333333333,-2.15));
#20834=CARTESIAN_POINT('Ctrl Pts',(1.86195461813654,3.61666666666666,-1.075));
#20835=CARTESIAN_POINT('Ctrl Pts',(2.48260615751539,3.67499999999999,-4.5604735265171E-16));
#20836=CARTESIAN_POINT('Ctrl Pts',(1.86195461813654,3.73333333333333,1.075));
#20837=CARTESIAN_POINT('Ctrl Pts',(1.2413030787577,3.79166666666666,2.15));
#20838=CARTESIAN_POINT('Ctrl Pts',(0.,3.84999999999999,2.15));
#20839=CARTESIAN_POINT('Ctrl Pts',(-1.2413030787577,3.90833333333333,2.15));
#20840=CARTESIAN_POINT('Ctrl Pts',(-1.86195461813654,3.96666666666666,1.075));
#20841=CARTESIAN_POINT('Ctrl Pts',(-2.48260615751539,4.02499999999999,1.52015784217237E-16));
#20842=CARTESIAN_POINT('Ctrl Pts',(-1.86195461813654,4.08333333333333,-1.075));
#20843=CARTESIAN_POINT('Ctrl Pts',(-1.2413030787577,4.14166666666666,-2.15));
#20844=CARTESIAN_POINT('Ctrl Pts',(-2.63299061816681E-16,4.19999999999999,
-2.15));
#20845=CARTESIAN_POINT('Ctrl Pts',(1.24130307875769,4.25833333333333,-2.15));
#20846=CARTESIAN_POINT('Ctrl Pts',(1.86195461813654,4.31666666666666,-1.075));
#20847=CARTESIAN_POINT('Ctrl Pts',(2.48260615751539,4.37499999999999,-4.5604735265171E-16));
#20848=CARTESIAN_POINT('Ctrl Pts',(1.86195461813654,4.43333333333333,1.075));
#20849=CARTESIAN_POINT('Ctrl Pts',(1.2413030787577,4.49166666666666,2.15));
#20850=CARTESIAN_POINT('Ctrl Pts',(0.,4.54999999999999,2.15));
#20851=CARTESIAN_POINT('Ctrl Pts',(0.,0.35,2.35502525316942));
#20852=CARTESIAN_POINT('Ctrl Pts',(-1.35967446386573,0.408333333333333,
2.35502525316942));
#20853=CARTESIAN_POINT('Ctrl Pts',(-2.03951169579859,0.466666666666666,
1.17751262658471));
#20854=CARTESIAN_POINT('Ctrl Pts',(-2.71934892773146,0.525,1.66512098005556E-16));
#20855=CARTESIAN_POINT('Ctrl Pts',(-2.03951169579859,0.583333333333333,
-1.17751262658471));
#20856=CARTESIAN_POINT('Ctrl Pts',(-1.35967446386573,0.641666666666666,
-2.35502525316942));
#20857=CARTESIAN_POINT('Ctrl Pts',(-2.88407413820511E-16,0.699999999999999,
-2.35502525316942));
#20858=CARTESIAN_POINT('Ctrl Pts',(1.35967446386573,0.758333333333333,-2.35502525316942));
#20859=CARTESIAN_POINT('Ctrl Pts',(2.03951169579859,0.816666666666666,-1.17751262658471));
#20860=CARTESIAN_POINT('Ctrl Pts',(2.71934892773146,0.874999999999999,-4.99536294016668E-16));
#20861=CARTESIAN_POINT('Ctrl Pts',(2.03951169579859,0.933333333333332,1.17751262658471));
#20862=CARTESIAN_POINT('Ctrl Pts',(1.35967446386573,0.991666666666665,2.35502525316942));
#20863=CARTESIAN_POINT('Ctrl Pts',(0.,1.05,2.35502525316942));
#20864=CARTESIAN_POINT('Ctrl Pts',(-1.35967446386573,1.10833333333333,2.35502525316942));
#20865=CARTESIAN_POINT('Ctrl Pts',(-2.03951169579859,1.16666666666666,1.17751262658471));
#20866=CARTESIAN_POINT('Ctrl Pts',(-2.71934892773146,1.225,1.66512098005556E-16));
#20867=CARTESIAN_POINT('Ctrl Pts',(-2.03951169579859,1.28333333333333,-1.17751262658471));
#20868=CARTESIAN_POINT('Ctrl Pts',(-1.35967446386573,1.34166666666667,-2.35502525316942));
#20869=CARTESIAN_POINT('Ctrl Pts',(-2.88407413820511E-16,1.4,-2.35502525316942));
#20870=CARTESIAN_POINT('Ctrl Pts',(1.35967446386573,1.45833333333333,-2.35502525316942));
#20871=CARTESIAN_POINT('Ctrl Pts',(2.03951169579859,1.51666666666666,-1.17751262658471));
#20872=CARTESIAN_POINT('Ctrl Pts',(2.71934892773146,1.575,-4.99536294016668E-16));
#20873=CARTESIAN_POINT('Ctrl Pts',(2.03951169579859,1.63333333333333,1.17751262658471));
#20874=CARTESIAN_POINT('Ctrl Pts',(1.35967446386573,1.69166666666666,2.35502525316942));
#20875=CARTESIAN_POINT('Ctrl Pts',(0.,1.75,2.35502525316942));
#20876=CARTESIAN_POINT('Ctrl Pts',(-1.35967446386573,1.80833333333333,2.35502525316942));
#20877=CARTESIAN_POINT('Ctrl Pts',(-2.03951169579859,1.86666666666666,1.17751262658471));
#20878=CARTESIAN_POINT('Ctrl Pts',(-2.71934892773146,1.925,1.66512098005556E-16));
#20879=CARTESIAN_POINT('Ctrl Pts',(-2.03951169579859,1.98333333333333,-1.17751262658471));
#20880=CARTESIAN_POINT('Ctrl Pts',(-1.35967446386573,2.04166666666666,-2.35502525316942));
#20881=CARTESIAN_POINT('Ctrl Pts',(-2.88407413820511E-16,2.1,-2.35502525316942));
#20882=CARTESIAN_POINT('Ctrl Pts',(1.35967446386573,2.15833333333333,-2.35502525316942));
#20883=CARTESIAN_POINT('Ctrl Pts',(2.03951169579859,2.21666666666666,-1.17751262658471));
#20884=CARTESIAN_POINT('Ctrl Pts',(2.71934892773146,2.275,-4.99536294016668E-16));
#20885=CARTESIAN_POINT('Ctrl Pts',(2.03951169579859,2.33333333333333,1.17751262658471));
#20886=CARTESIAN_POINT('Ctrl Pts',(1.35967446386573,2.39166666666666,2.35502525316942));
#20887=CARTESIAN_POINT('Ctrl Pts',(0.,2.45,2.35502525316942));
#20888=CARTESIAN_POINT('Ctrl Pts',(-1.35967446386573,2.50833333333333,2.35502525316942));
#20889=CARTESIAN_POINT('Ctrl Pts',(-2.03951169579859,2.56666666666666,1.17751262658471));
#20890=CARTESIAN_POINT('Ctrl Pts',(-2.71934892773146,2.62499999999999,1.66512098005556E-16));
#20891=CARTESIAN_POINT('Ctrl Pts',(-2.03951169579859,2.68333333333333,-1.17751262658471));
#20892=CARTESIAN_POINT('Ctrl Pts',(-1.35967446386573,2.74166666666666,-2.35502525316942));
#20893=CARTESIAN_POINT('Ctrl Pts',(-2.88407413820511E-16,2.8,-2.35502525316942));
#20894=CARTESIAN_POINT('Ctrl Pts',(1.35967446386573,2.85833333333333,-2.35502525316942));
#20895=CARTESIAN_POINT('Ctrl Pts',(2.03951169579859,2.91666666666666,-1.17751262658471));
#20896=CARTESIAN_POINT('Ctrl Pts',(2.71934892773146,2.97499999999999,-4.99536294016668E-16));
#20897=CARTESIAN_POINT('Ctrl Pts',(2.03951169579859,3.03333333333333,1.17751262658471));
#20898=CARTESIAN_POINT('Ctrl Pts',(1.35967446386573,3.09166666666666,2.35502525316942));
#20899=CARTESIAN_POINT('Ctrl Pts',(0.,3.14999999999999,2.35502525316942));
#20900=CARTESIAN_POINT('Ctrl Pts',(-1.35967446386573,3.20833333333333,2.35502525316942));
#20901=CARTESIAN_POINT('Ctrl Pts',(-2.03951169579859,3.26666666666666,1.17751262658471));
#20902=CARTESIAN_POINT('Ctrl Pts',(-2.71934892773146,3.32499999999999,1.66512098005556E-16));
#20903=CARTESIAN_POINT('Ctrl Pts',(-2.03951169579859,3.38333333333333,-1.17751262658471));
#20904=CARTESIAN_POINT('Ctrl Pts',(-1.35967446386573,3.44166666666666,-2.35502525316942));
#20905=CARTESIAN_POINT('Ctrl Pts',(-2.88407413820511E-16,3.49999999999999,
-2.35502525316942));
#20906=CARTESIAN_POINT('Ctrl Pts',(1.35967446386573,3.55833333333333,-2.35502525316942));
#20907=CARTESIAN_POINT('Ctrl Pts',(2.03951169579859,3.61666666666666,-1.17751262658471));
#20908=CARTESIAN_POINT('Ctrl Pts',(2.71934892773146,3.67499999999999,-4.99536294016668E-16));
#20909=CARTESIAN_POINT('Ctrl Pts',(2.03951169579859,3.73333333333333,1.17751262658471));
#20910=CARTESIAN_POINT('Ctrl Pts',(1.35967446386573,3.79166666666666,2.35502525316942));
#20911=CARTESIAN_POINT('Ctrl Pts',(0.,3.84999999999999,2.35502525316942));
#20912=CARTESIAN_POINT('Ctrl Pts',(-1.35967446386573,3.90833333333333,2.35502525316942));
#20913=CARTESIAN_POINT('Ctrl Pts',(-2.03951169579859,3.96666666666666,1.17751262658471));
#20914=CARTESIAN_POINT('Ctrl Pts',(-2.71934892773146,4.02499999999999,1.66512098005556E-16));
#20915=CARTESIAN_POINT('Ctrl Pts',(-2.03951169579859,4.08333333333333,-1.17751262658471));
#20916=CARTESIAN_POINT('Ctrl Pts',(-1.35967446386573,4.14166666666666,-2.35502525316942));
#20917=CARTESIAN_POINT('Ctrl Pts',(-2.88407413820511E-16,4.19999999999999,
-2.35502525316942));
#20918=CARTESIAN_POINT('Ctrl Pts',(1.35967446386573,4.25833333333332,-2.35502525316942));
#20919=CARTESIAN_POINT('Ctrl Pts',(2.03951169579859,4.31666666666666,-1.17751262658471));
#20920=CARTESIAN_POINT('Ctrl Pts',(2.71934892773146,4.37499999999999,-4.99536294016668E-16));
#20921=CARTESIAN_POINT('Ctrl Pts',(2.03951169579859,4.43333333333332,1.17751262658471));
#20922=CARTESIAN_POINT('Ctrl Pts',(1.35967446386573,4.49166666666666,2.35502525316942));
#20923=CARTESIAN_POINT('Ctrl Pts',(0.,4.54999999999999,2.35502525316942));
#20924=CARTESIAN_POINT('Ctrl Pts',(0.,0.205025253169417,2.5));
#20925=CARTESIAN_POINT('Ctrl Pts',(-1.44337567297406,0.26335858650275,2.5));
#20926=CARTESIAN_POINT('Ctrl Pts',(-2.1650635094611,0.321691919836083,1.25));
#20927=CARTESIAN_POINT('Ctrl Pts',(-2.88675134594813,0.380025253169416,
1.76762539787484E-16));
#20928=CARTESIAN_POINT('Ctrl Pts',(-2.1650635094611,0.43835858650275,-1.25));
#20929=CARTESIAN_POINT('Ctrl Pts',(-1.44337567297407,0.496691919836083,
-2.5));
#20930=CARTESIAN_POINT('Ctrl Pts',(-3.06161699786838E-16,0.555025253169416,
-2.5));
#20931=CARTESIAN_POINT('Ctrl Pts',(1.44337567297406,0.613358586502749,-2.5));
#20932=CARTESIAN_POINT('Ctrl Pts',(2.1650635094611,0.671691919836083,-1.25));
#20933=CARTESIAN_POINT('Ctrl Pts',(2.88675134594813,0.730025253169416,-5.30287619362453E-16));
#20934=CARTESIAN_POINT('Ctrl Pts',(2.1650635094611,0.788358586502749,1.25));
#20935=CARTESIAN_POINT('Ctrl Pts',(1.44337567297407,0.846691919836082,2.5));
#20936=CARTESIAN_POINT('Ctrl Pts',(0.,0.905025253169415,2.5));
#20937=CARTESIAN_POINT('Ctrl Pts',(-1.44337567297406,0.963358586502749,
2.5));
#20938=CARTESIAN_POINT('Ctrl Pts',(-2.1650635094611,1.02169191983608,1.25));
#20939=CARTESIAN_POINT('Ctrl Pts',(-2.88675134594813,1.08002525316942,1.76762539787484E-16));
#20940=CARTESIAN_POINT('Ctrl Pts',(-2.1650635094611,1.13835858650275,-1.25));
#20941=CARTESIAN_POINT('Ctrl Pts',(-1.44337567297407,1.19669191983608,-2.5));
#20942=CARTESIAN_POINT('Ctrl Pts',(-3.06161699786838E-16,1.25502525316941,
-2.5));
#20943=CARTESIAN_POINT('Ctrl Pts',(1.44337567297406,1.31335858650275,-2.5));
#20944=CARTESIAN_POINT('Ctrl Pts',(2.1650635094611,1.37169191983608,-1.25));
#20945=CARTESIAN_POINT('Ctrl Pts',(2.88675134594813,1.43002525316941,-5.30287619362453E-16));
#20946=CARTESIAN_POINT('Ctrl Pts',(2.1650635094611,1.48835858650275,1.25));
#20947=CARTESIAN_POINT('Ctrl Pts',(1.44337567297407,1.54669191983608,2.5));
#20948=CARTESIAN_POINT('Ctrl Pts',(0.,1.60502525316941,2.5));
#20949=CARTESIAN_POINT('Ctrl Pts',(-1.44337567297406,1.66335858650275,2.5));
#20950=CARTESIAN_POINT('Ctrl Pts',(-2.1650635094611,1.72169191983608,1.25));
#20951=CARTESIAN_POINT('Ctrl Pts',(-2.88675134594813,1.78002525316941,1.76762539787484E-16));
#20952=CARTESIAN_POINT('Ctrl Pts',(-2.1650635094611,1.83835858650275,-1.25));
#20953=CARTESIAN_POINT('Ctrl Pts',(-1.44337567297407,1.89669191983608,-2.5));
#20954=CARTESIAN_POINT('Ctrl Pts',(-3.06161699786838E-16,1.95502525316941,
-2.5));
#20955=CARTESIAN_POINT('Ctrl Pts',(1.44337567297406,2.01335858650275,-2.5));
#20956=CARTESIAN_POINT('Ctrl Pts',(2.1650635094611,2.07169191983608,-1.25));
#20957=CARTESIAN_POINT('Ctrl Pts',(2.88675134594813,2.13002525316941,-5.30287619362453E-16));
#20958=CARTESIAN_POINT('Ctrl Pts',(2.1650635094611,2.18835858650275,1.25));
#20959=CARTESIAN_POINT('Ctrl Pts',(1.44337567297407,2.24669191983608,2.5));
#20960=CARTESIAN_POINT('Ctrl Pts',(0.,2.30502525316941,2.5));
#20961=CARTESIAN_POINT('Ctrl Pts',(-1.44337567297406,2.36335858650275,2.5));
#20962=CARTESIAN_POINT('Ctrl Pts',(-2.1650635094611,2.42169191983608,1.25));
#20963=CARTESIAN_POINT('Ctrl Pts',(-2.88675134594813,2.48002525316941,1.76762539787484E-16));
#20964=CARTESIAN_POINT('Ctrl Pts',(-2.1650635094611,2.53835858650275,-1.25));
#20965=CARTESIAN_POINT('Ctrl Pts',(-1.44337567297407,2.59669191983608,-2.5));
#20966=CARTESIAN_POINT('Ctrl Pts',(-3.06161699786838E-16,2.65502525316941,
-2.5));
#20967=CARTESIAN_POINT('Ctrl Pts',(1.44337567297406,2.71335858650274,-2.5));
#20968=CARTESIAN_POINT('Ctrl Pts',(2.1650635094611,2.77169191983608,-1.25));
#20969=CARTESIAN_POINT('Ctrl Pts',(2.88675134594813,2.83002525316941,-5.30287619362453E-16));
#20970=CARTESIAN_POINT('Ctrl Pts',(2.1650635094611,2.88835858650274,1.25));
#20971=CARTESIAN_POINT('Ctrl Pts',(1.44337567297407,2.94669191983608,2.5));
#20972=CARTESIAN_POINT('Ctrl Pts',(0.,3.00502525316941,2.5));
#20973=CARTESIAN_POINT('Ctrl Pts',(-1.44337567297406,3.06335858650274,2.5));
#20974=CARTESIAN_POINT('Ctrl Pts',(-2.1650635094611,3.12169191983608,1.25));
#20975=CARTESIAN_POINT('Ctrl Pts',(-2.88675134594813,3.18002525316941,1.76762539787484E-16));
#20976=CARTESIAN_POINT('Ctrl Pts',(-2.1650635094611,3.23835858650274,-1.25));
#20977=CARTESIAN_POINT('Ctrl Pts',(-1.44337567297407,3.29669191983608,-2.5));
#20978=CARTESIAN_POINT('Ctrl Pts',(-3.06161699786838E-16,3.35502525316941,
-2.5));
#20979=CARTESIAN_POINT('Ctrl Pts',(1.44337567297406,3.41335858650274,-2.5));
#20980=CARTESIAN_POINT('Ctrl Pts',(2.1650635094611,3.47169191983608,-1.25));
#20981=CARTESIAN_POINT('Ctrl Pts',(2.88675134594813,3.53002525316941,-5.30287619362453E-16));
#20982=CARTESIAN_POINT('Ctrl Pts',(2.1650635094611,3.58835858650274,1.25));
#20983=CARTESIAN_POINT('Ctrl Pts',(1.44337567297407,3.64669191983608,2.5));
#20984=CARTESIAN_POINT('Ctrl Pts',(0.,3.70502525316941,2.5));
#20985=CARTESIAN_POINT('Ctrl Pts',(-1.44337567297406,3.76335858650274,2.5));
#20986=CARTESIAN_POINT('Ctrl Pts',(-2.1650635094611,3.82169191983608,1.25));
#20987=CARTESIAN_POINT('Ctrl Pts',(-2.88675134594813,3.88002525316941,1.76762539787484E-16));
#20988=CARTESIAN_POINT('Ctrl Pts',(-2.1650635094611,3.93835858650274,-1.25));
#20989=CARTESIAN_POINT('Ctrl Pts',(-1.44337567297407,3.99669191983608,-2.5));
#20990=CARTESIAN_POINT('Ctrl Pts',(-3.06161699786838E-16,4.05502525316941,
-2.5));
#20991=CARTESIAN_POINT('Ctrl Pts',(1.44337567297406,4.11335858650274,-2.5));
#20992=CARTESIAN_POINT('Ctrl Pts',(2.1650635094611,4.17169191983608,-1.25));
#20993=CARTESIAN_POINT('Ctrl Pts',(2.88675134594813,4.23002525316941,-5.30287619362453E-16));
#20994=CARTESIAN_POINT('Ctrl Pts',(2.1650635094611,4.28835858650274,1.25));
#20995=CARTESIAN_POINT('Ctrl Pts',(1.44337567297407,4.34669191983608,2.5));
#20996=CARTESIAN_POINT('Ctrl Pts',(0.,4.40502525316941,2.5));
#20997=CARTESIAN_POINT('Ctrl Pts',(0.,4.28626379701574E-17,2.5));
#20998=CARTESIAN_POINT('Ctrl Pts',(-1.44337567297406,0.0583333333333333,
2.5));
#20999=CARTESIAN_POINT('Ctrl Pts',(-2.1650635094611,0.116666666666666,1.25));
#21000=CARTESIAN_POINT('Ctrl Pts',(-2.88675134594813,0.175,1.76762539787484E-16));
#21001=CARTESIAN_POINT('Ctrl Pts',(-2.1650635094611,0.233333333333333,-1.25));
#21002=CARTESIAN_POINT('Ctrl Pts',(-1.44337567297407,0.291666666666666,
-2.5));
#21003=CARTESIAN_POINT('Ctrl Pts',(-3.06161699786838E-16,0.349999999999999,
-2.5));
#21004=CARTESIAN_POINT('Ctrl Pts',(1.44337567297406,0.408333333333333,-2.5));
#21005=CARTESIAN_POINT('Ctrl Pts',(2.1650635094611,0.466666666666666,-1.25));
#21006=CARTESIAN_POINT('Ctrl Pts',(2.88675134594813,0.524999999999999,-5.30287619362453E-16));
#21007=CARTESIAN_POINT('Ctrl Pts',(2.1650635094611,0.583333333333332,1.25));
#21008=CARTESIAN_POINT('Ctrl Pts',(1.44337567297407,0.641666666666665,2.5));
#21009=CARTESIAN_POINT('Ctrl Pts',(0.,0.699999999999999,2.5));
#21010=CARTESIAN_POINT('Ctrl Pts',(-1.44337567297406,0.758333333333332,
2.5));
#21011=CARTESIAN_POINT('Ctrl Pts',(-2.1650635094611,0.816666666666665,1.25));
#21012=CARTESIAN_POINT('Ctrl Pts',(-2.88675134594813,0.874999999999998,
1.76762539787484E-16));
#21013=CARTESIAN_POINT('Ctrl Pts',(-2.1650635094611,0.933333333333332,-1.25));
#21014=CARTESIAN_POINT('Ctrl Pts',(-1.44337567297407,0.991666666666665,
-2.5));
#21015=CARTESIAN_POINT('Ctrl Pts',(-3.06161699786838E-16,1.05,-2.5));
#21016=CARTESIAN_POINT('Ctrl Pts',(1.44337567297406,1.10833333333333,-2.5));
#21017=CARTESIAN_POINT('Ctrl Pts',(2.1650635094611,1.16666666666666,-1.25));
#21018=CARTESIAN_POINT('Ctrl Pts',(2.88675134594813,1.225,-5.30287619362453E-16));
#21019=CARTESIAN_POINT('Ctrl Pts',(2.1650635094611,1.28333333333333,1.25));
#21020=CARTESIAN_POINT('Ctrl Pts',(1.44337567297407,1.34166666666666,2.5));
#21021=CARTESIAN_POINT('Ctrl Pts',(0.,1.4,2.5));
#21022=CARTESIAN_POINT('Ctrl Pts',(-1.44337567297406,1.45833333333333,2.5));
#21023=CARTESIAN_POINT('Ctrl Pts',(-2.1650635094611,1.51666666666666,1.25));
#21024=CARTESIAN_POINT('Ctrl Pts',(-2.88675134594813,1.575,1.76762539787484E-16));
#21025=CARTESIAN_POINT('Ctrl Pts',(-2.1650635094611,1.63333333333333,-1.25));
#21026=CARTESIAN_POINT('Ctrl Pts',(-1.44337567297407,1.69166666666666,-2.5));
#21027=CARTESIAN_POINT('Ctrl Pts',(-3.06161699786838E-16,1.75,-2.5));
#21028=CARTESIAN_POINT('Ctrl Pts',(1.44337567297406,1.80833333333333,-2.5));
#21029=CARTESIAN_POINT('Ctrl Pts',(2.1650635094611,1.86666666666666,-1.25));
#21030=CARTESIAN_POINT('Ctrl Pts',(2.88675134594813,1.925,-5.30287619362453E-16));
#21031=CARTESIAN_POINT('Ctrl Pts',(2.1650635094611,1.98333333333333,1.25));
#21032=CARTESIAN_POINT('Ctrl Pts',(1.44337567297407,2.04166666666666,2.5));
#21033=CARTESIAN_POINT('Ctrl Pts',(0.,2.1,2.5));
#21034=CARTESIAN_POINT('Ctrl Pts',(-1.44337567297406,2.15833333333333,2.5));
#21035=CARTESIAN_POINT('Ctrl Pts',(-2.1650635094611,2.21666666666666,1.25));
#21036=CARTESIAN_POINT('Ctrl Pts',(-2.88675134594813,2.275,1.76762539787484E-16));
#21037=CARTESIAN_POINT('Ctrl Pts',(-2.1650635094611,2.33333333333333,-1.25));
#21038=CARTESIAN_POINT('Ctrl Pts',(-1.44337567297407,2.39166666666666,-2.5));
#21039=CARTESIAN_POINT('Ctrl Pts',(-3.06161699786838E-16,2.45,-2.5));
#21040=CARTESIAN_POINT('Ctrl Pts',(1.44337567297406,2.50833333333333,-2.5));
#21041=CARTESIAN_POINT('Ctrl Pts',(2.1650635094611,2.56666666666666,-1.25));
#21042=CARTESIAN_POINT('Ctrl Pts',(2.88675134594813,2.62499999999999,-5.30287619362453E-16));
#21043=CARTESIAN_POINT('Ctrl Pts',(2.1650635094611,2.68333333333333,1.25));
#21044=CARTESIAN_POINT('Ctrl Pts',(1.44337567297407,2.74166666666666,2.5));
#21045=CARTESIAN_POINT('Ctrl Pts',(0.,2.79999999999999,2.5));
#21046=CARTESIAN_POINT('Ctrl Pts',(-1.44337567297406,2.85833333333333,2.5));
#21047=CARTESIAN_POINT('Ctrl Pts',(-2.1650635094611,2.91666666666666,1.25));
#21048=CARTESIAN_POINT('Ctrl Pts',(-2.88675134594813,2.97499999999999,1.76762539787484E-16));
#21049=CARTESIAN_POINT('Ctrl Pts',(-2.1650635094611,3.03333333333333,-1.25));
#21050=CARTESIAN_POINT('Ctrl Pts',(-1.44337567297407,3.09166666666666,-2.5));
#21051=CARTESIAN_POINT('Ctrl Pts',(-3.06161699786838E-16,3.14999999999999,
-2.5));
#21052=CARTESIAN_POINT('Ctrl Pts',(1.44337567297406,3.20833333333333,-2.5));
#21053=CARTESIAN_POINT('Ctrl Pts',(2.1650635094611,3.26666666666666,-1.25));
#21054=CARTESIAN_POINT('Ctrl Pts',(2.88675134594813,3.32499999999999,-5.30287619362453E-16));
#21055=CARTESIAN_POINT('Ctrl Pts',(2.1650635094611,3.38333333333333,1.25));
#21056=CARTESIAN_POINT('Ctrl Pts',(1.44337567297407,3.44166666666666,2.5));
#21057=CARTESIAN_POINT('Ctrl Pts',(0.,3.49999999999999,2.5));
#21058=CARTESIAN_POINT('Ctrl Pts',(-1.44337567297406,3.55833333333333,2.5));
#21059=CARTESIAN_POINT('Ctrl Pts',(-2.1650635094611,3.61666666666666,1.25));
#21060=CARTESIAN_POINT('Ctrl Pts',(-2.88675134594813,3.67499999999999,1.76762539787484E-16));
#21061=CARTESIAN_POINT('Ctrl Pts',(-2.1650635094611,3.73333333333333,-1.25));
#21062=CARTESIAN_POINT('Ctrl Pts',(-1.44337567297407,3.79166666666666,-2.5));
#21063=CARTESIAN_POINT('Ctrl Pts',(-3.06161699786838E-16,3.84999999999999,
-2.5));
#21064=CARTESIAN_POINT('Ctrl Pts',(1.44337567297406,3.90833333333333,-2.5));
#21065=CARTESIAN_POINT('Ctrl Pts',(2.1650635094611,3.96666666666666,-1.25));
#21066=CARTESIAN_POINT('Ctrl Pts',(2.88675134594813,4.02499999999999,-5.30287619362453E-16));
#21067=CARTESIAN_POINT('Ctrl Pts',(2.1650635094611,4.08333333333333,1.25));
#21068=CARTESIAN_POINT('Ctrl Pts',(1.44337567297407,4.14166666666666,2.5));
#21069=CARTESIAN_POINT('Ctrl Pts',(0.,4.19999999999999,2.5));
#21070=CARTESIAN_POINT('Origin',(0.,0.,2.15));
#21071=CARTESIAN_POINT('Origin',(-1.80160437084306E-13,4.2,2.15));
#21072=CARTESIAN_POINT('Origin',(-1.80160437084306E-13,4.2,2.15));
#21073=CARTESIAN_POINT('Origin',(0.,0.,2.15));
#21074=CARTESIAN_POINT('',(0.,0.,0.));
#21075=CARTESIAN_POINT('Origin',(0.,0.,0.));
#21076=CARTESIAN_POINT('',(-2.75,1.52655665885959E-16,-1.68388934882762E-16));
#21077=CARTESIAN_POINT('',(2.75,-1.52655665885959E-16,-1.6838893488276E-16));
#21078=CARTESIAN_POINT('Origin',(0.,0.,0.));
#21079=CARTESIAN_POINT('',(0.,0.,0.));
#21080=CARTESIAN_POINT('',(-3.37971241867727,13.95,2.51789857617014));
#21081=CARTESIAN_POINT('',(10.9,13.85,0.));
#21082=CARTESIAN_POINT('',(6.86994557784279E-15,7.89999999999998,5.148143654755E-15));
#21083=CARTESIAN_POINT('',(-2.50000000000005,13.8,1.74574066942157E-14));
#21084=CARTESIAN_POINT('',(5.85000000000003,-7.99999999999997,-9.38988789986312E-16));
#21085=CARTESIAN_POINT('',(0.900000000000024,-7.99999999999999,2.43086292165551E-16));
#21086=CARTESIAN_POINT('',(4.49999999999991,13.8,1.80517764902569E-15));
#21087=CARTESIAN_POINT('',(0.,0.,0.));
#21088=CARTESIAN_POINT('Origin',(0.,0.,0.));
#21089=CARTESIAN_POINT('',(-8.45006291411674E-16,2.02066721859313E-16,-6.9));
#21090=CARTESIAN_POINT('Origin',(-1.04707301327099E-15,0.,-8.55));
#21091=CARTESIAN_POINT('Origin',(0.,-2.02066721859313E-16,0.));
#21092=CARTESIAN_POINT('',(0.,0.,0.));
#21093=CARTESIAN_POINT('',(0.,0.,0.));
#21094=CARTESIAN_POINT('Origin',(0.,275.,0.));
#21095=CARTESIAN_POINT('',(-1.35935794705356E-15,13.9512489600659,11.1));
#21096=CARTESIAN_POINT('Origin',(0.,13.9512489600658,0.));
#21097=CARTESIAN_POINT('',(-9.5723472968307E-16,32.7351817276402,11.1));
#21098=CARTESIAN_POINT('',(-1.35935794705356E-15,275.,11.1));
#21099=CARTESIAN_POINT('',(-1.5009622134597,34.2419663837872,10.9980503923998));
#21100=CARTESIAN_POINT('Ctrl Pts',(-1.5009622134597,34.2419663837872,10.9980503923998));
#21101=CARTESIAN_POINT('Ctrl Pts',(-1.5009622134597,34.0448673617028,10.9980503923998));
#21102=CARTESIAN_POINT('Ctrl Pts',(-1.4771810723556,33.8362237308831,11.001402687493));
#21103=CARTESIAN_POINT('Ctrl Pts',(-1.38530410221155,33.5102351295637,11.0132837659748));
#21104=CARTESIAN_POINT('Ctrl Pts',(-1.33034819384694,33.3781157666075,11.0202692332752));
#21105=CARTESIAN_POINT('Ctrl Pts',(-1.18533576935023,33.1591718022942,11.036735456266));
#21106=CARTESIAN_POINT('Ctrl Pts',(-1.10400652085937,33.0725369802661,11.0453977168056));
#21107=CARTESIAN_POINT('Ctrl Pts',(-0.892079326680414,32.9165975969895,
11.0646884672856));
#21108=CARTESIAN_POINT('Ctrl Pts',(-0.763175852377866,32.858361072496,11.0745648140582));
#21109=CARTESIAN_POINT('Ctrl Pts',(-0.521393923343649,32.7862330357377,
11.0882585321735));
#21110=CARTESIAN_POINT('Ctrl Pts',(-0.410221375913272,32.7652602373854,
11.0929635501988));
#21111=CARTESIAN_POINT('Ctrl Pts',(-0.245516803362297,32.7459057253595,
11.0974190600975));
#21112=CARTESIAN_POINT('Ctrl Pts',(-0.190368819985243,32.741377542263,11.0985035405639));
#21113=CARTESIAN_POINT('Ctrl Pts',(-0.0911928932145138,32.7363522396234,
11.0997134708045));
#21114=CARTESIAN_POINT('Ctrl Pts',(-0.0467732754157406,32.7352238081385,
11.0999897520302));
#21115=CARTESIAN_POINT('Ctrl Pts',(-0.00166591943505573,32.735182112509,
11.0999999064775));
#21116=CARTESIAN_POINT('Ctrl Pts',(-0.000832984580003692,32.7351817276402,
11.1));
#21117=CARTESIAN_POINT('Ctrl Pts',(-5.55111512312578E-16,32.7351817276402,
11.1));
#21118=CARTESIAN_POINT('',(-1.5009622134597,71.2419663837872,10.9980503923998));
#21119=CARTESIAN_POINT('',(-1.5009622134597,52.7419663837872,10.9980503923998));
#21120=CARTESIAN_POINT('',(-2.62256926662081E-15,72.7487510399342,11.1));
#21121=CARTESIAN_POINT('Ctrl Pts',(-3.33066907387547E-15,72.7487510399342,
11.1));
#21122=CARTESIAN_POINT('Ctrl Pts',(-0.0431795099645684,72.7487510399342,
11.1));
#21123=CARTESIAN_POINT('Ctrl Pts',(-0.0864912359924271,72.7477167835041,
11.0997467925512));
#21124=CARTESIAN_POINT('Ctrl Pts',(-0.183646082354134,72.7430091857572,
11.0986122679057));
#21125=CARTESIAN_POINT('Ctrl Pts',(-0.237861556176835,72.7387110754265,
11.0975813610593));
#21126=CARTESIAN_POINT('Ctrl Pts',(-0.396947158377275,72.7206077607173,
11.093400647027));
#21127=CARTESIAN_POINT('Ctrl Pts',(-0.503286882970604,72.7013249659842,
11.0890555714104));
#21128=CARTESIAN_POINT('Ctrl Pts',(-0.733608402260413,72.6362267971513,
11.0764757024731));
#21129=CARTESIAN_POINT('Ctrl Pts',(-0.857006401108304,72.5843799091735,
11.0674274747807));
#21130=CARTESIAN_POINT('Ctrl Pts',(-1.0699564859103,72.4419884523097,11.0487859403242));
#21131=CARTESIAN_POINT('Ctrl Pts',(-1.15605156955383,72.358608719571,11.0398711384066));
#21132=CARTESIAN_POINT('Ctrl Pts',(-1.30730179997395,72.1488438578608,11.0230378127299));
#21133=CARTESIAN_POINT('Ctrl Pts',(-1.36488506375574,72.0245694303452,11.0158446286986));
#21134=CARTESIAN_POINT('Ctrl Pts',(-1.47430578438809,71.6831286857258,11.0018689838731));
#21135=CARTESIAN_POINT('Ctrl Pts',(-1.5009622134597,71.4507884295538,10.9980503923998));
#21136=CARTESIAN_POINT('Ctrl Pts',(-1.5009622134597,71.2419663837872,10.9980503923998));
#21137=CARTESIAN_POINT('',(0.,75.4487510399342,11.1));
#21138=CARTESIAN_POINT('',(-1.35935794705356E-15,275.,11.1));
#21139=CARTESIAN_POINT('Origin',(0.,75.4487510399342,0.));
#21140=CARTESIAN_POINT('',(1.5009622134597,71.2419663837872,10.9980503923998));
#21141=CARTESIAN_POINT('Ctrl Pts',(1.5009622134597,71.2419663837872,10.9980503923998));
#21142=CARTESIAN_POINT('Ctrl Pts',(1.5009622134597,71.4504917689704,10.9980503923998));
#21143=CARTESIAN_POINT('Ctrl Pts',(1.47434652131067,71.672803365615,11.0018223294187));
#21144=CARTESIAN_POINT('Ctrl Pts',(1.37309027919535,72.0047784777117,11.0148201900203));
#21145=CARTESIAN_POINT('Ctrl Pts',(1.31654601035472,72.1320608146007,11.0219331133145));
#21146=CARTESIAN_POINT('Ctrl Pts',(1.16784203699473,72.345327367031,11.0386176428475));
#21147=CARTESIAN_POINT('Ctrl Pts',(1.0837084064114,72.4299633960732,11.0474297365141));
#21148=CARTESIAN_POINT('Ctrl Pts',(0.871159298255555,72.5776598312476,11.0663360902504));
#21149=CARTESIAN_POINT('Ctrl Pts',(0.745523925005296,72.6320095746663,11.0757141514867));
#21150=CARTESIAN_POINT('Ctrl Pts',(0.512543745213089,72.6993182274867,11.088629433639));
#21151=CARTESIAN_POINT('Ctrl Pts',(0.406386833752675,72.7190769495851,11.0930577318951));
#21152=CARTESIAN_POINT('Ctrl Pts',(0.246410373793648,72.7379457354566,11.0973997874919));
#21153=CARTESIAN_POINT('Ctrl Pts',(0.191151023811988,72.7425013416222,11.0984906444422));
#21154=CARTESIAN_POINT('Ctrl Pts',(0.0918578103499711,72.7475581223538,
11.0997080150118));
#21155=CARTESIAN_POINT('Ctrl Pts',(0.0474310645609758,72.7486976181121,
11.0999869901433));
#21156=CARTESIAN_POINT('Ctrl Pts',(0.00209958546977268,72.7487504285997,
11.0999998514453));
#21157=CARTESIAN_POINT('Ctrl Pts',(0.00104983181341904,72.7487510399342,
11.1));
#21158=CARTESIAN_POINT('Ctrl Pts',(-3.33066907387547E-15,72.7487510399342,
11.1));
#21159=CARTESIAN_POINT('',(1.5009622134597,34.2419663837872,10.9980503923998));
#21160=CARTESIAN_POINT('',(1.5009622134597,52.7419663837872,10.9980503923998));
#21161=CARTESIAN_POINT('Ctrl Pts',(-5.55111512312578E-16,32.7351817276402,
11.1));
#21162=CARTESIAN_POINT('Ctrl Pts',(0.0434004817053344,32.7351817276402,
11.1));
#21163=CARTESIAN_POINT('Ctrl Pts',(0.0869359496621808,32.7362265936286,
11.0997441811035));
#21164=CARTESIAN_POINT('Ctrl Pts',(0.18441610004499,32.7409747471531,11.0986000062274));
#21165=CARTESIAN_POINT('Ctrl Pts',(0.238736148222327,32.7452987075796,11.0975630731579));
#21166=CARTESIAN_POINT('Ctrl Pts',(0.398446951974643,32.7635405469734,11.0933518720784));
#21167=CARTESIAN_POINT('Ctrl Pts',(0.505323294057922,32.7830083481295,11.0889673028681));
#21168=CARTESIAN_POINT('Ctrl Pts',(0.736910254577693,32.8488643339236,11.0762658297061));
#21169=CARTESIAN_POINT('Ctrl Pts',(0.860930452663077,32.9013952313581,11.0671267518481));
#21170=CARTESIAN_POINT('Ctrl Pts',(1.07377070841953,33.0452362980269,11.0484114414186));
#21171=CARTESIAN_POINT('Ctrl Pts',(1.15931674222104,33.1289571391808,11.0395252155594));
#21172=CARTESIAN_POINT('Ctrl Pts',(1.30985683194324,33.3396669565376,11.0227332589662));
#21173=CARTESIAN_POINT('Ctrl Pts',(1.36715456694082,33.4647551607029,11.0155618965373));
#21174=CARTESIAN_POINT('Ctrl Pts',(1.47298429182855,33.7994478579454,11.0020260798964));
#21175=CARTESIAN_POINT('Ctrl Pts',(1.5009622134597,34.0281657983113,10.9980503923998));
#21176=CARTESIAN_POINT('Ctrl Pts',(1.5009622134597,34.2419663837872,10.9980503923998));
#21177=CARTESIAN_POINT('',(-9.99594466036059,34.2419663837872,-4.82608437006737));
#21178=CARTESIAN_POINT('',(-10.923590324108,34.2419663837872,-1.97108458242009));
#21179=CARTESIAN_POINT('Ctrl Pts',(-9.99594466036059,34.2419663837872,-4.82608437006737));
#21180=CARTESIAN_POINT('Ctrl Pts',(-9.99594466036059,34.0448673617033,-4.82608437006737));
#21181=CARTESIAN_POINT('Ctrl Pts',(-10.0064816592001,33.8362237308843,-4.80450307700966));
#21182=CARTESIAN_POINT('Ctrl Pts',(-10.0461727814766,33.5102351295654,-4.72079434101999));
#21183=CARTESIAN_POINT('Ctrl Pts',(-10.0697986652978,33.3781157666092,-4.6706867943708));
#21184=CARTESIAN_POINT('Ctrl Pts',(-10.1302702775366,33.1591718022959,-4.53786012584765));
#21185=CARTESIAN_POINT('Ctrl Pts',(-10.1636406967919,33.0725369802679,-4.46318819982197));
#21186=CARTESIAN_POINT('Ctrl Pts',(-10.2474763953116,32.9165975969906,-4.26759463055083));
#21187=CARTESIAN_POINT('Ctrl Pts',(-10.2967027234606,32.8583610724967,-4.14805210033697));
#21188=CARTESIAN_POINT('Ctrl Pts',(-10.3844409483111,32.786233035738,-3.92233541281966));
#21189=CARTESIAN_POINT('Ctrl Pts',(-10.4232698928274,32.7652602373856,-3.81805796768108));
#21190=CARTESIAN_POINT('Ctrl Pts',(-10.4784038465197,32.7459057253596,-3.66279143896971));
#21191=CARTESIAN_POINT('Ctrl Pts',(-10.4964769128031,32.741377542263,-3.61067771291264));
#21192=CARTESIAN_POINT('Ctrl Pts',(-10.5282746716481,32.7363522396233,-3.51672969050312));
#21193=CARTESIAN_POINT('Ctrl Pts',(-10.5422638474917,32.7352238081385,-3.47456949913784));
#21194=CARTESIAN_POINT('Ctrl Pts',(-10.5696315831627,32.7351419995549,-3.39040474326441));
#21195=CARTESIAN_POINT('Ctrl Pts',(-10.5831009478896,32.7361860749744,-3.34812273992118));
#21196=CARTESIAN_POINT('Ctrl Pts',(-10.6123835666263,32.7409747471531,-3.25426588203641));
#21197=CARTESIAN_POINT('Ctrl Pts',(-10.6281832026957,32.7452987075796,-3.20228401631138));
#21198=CARTESIAN_POINT('Ctrl Pts',(-10.6735314650123,32.7635405469733,-3.04908868297999));
#21199=CARTESIAN_POINT('Ctrl Pts',(-10.702388097894,32.7830083481294,-2.94608833500493));
#21200=CARTESIAN_POINT('Ctrl Pts',(-10.7618725855528,32.8488643339231,-2.72191107605337));
#21201=CARTESIAN_POINT('Ctrl Pts',(-10.7915051548571,32.9013952313574,-2.60113672814137));
#21202=CARTESIAN_POINT('Ctrl Pts',(-10.8394770930345,33.0452362980253,-2.39293026699688));
#21203=CARTESIAN_POINT('Ctrl Pts',(-10.8574609682719,33.1289571391788,-2.30882515930038));
#21204=CARTESIAN_POINT('Ctrl Pts',(-10.8880103145914,33.339666956535,-2.16046402605025));
#21205=CARTESIAN_POINT('Ctrl Pts',(-10.8988959174762,33.4647551606998,-2.10375456894849));
#21206=CARTESIAN_POINT('Ctrl Pts',(-10.918725774357,33.7994478579428,-1.99892172210077));
#21207=CARTESIAN_POINT('Ctrl Pts',(-10.923590324108,34.0281657983102,-1.97108458242009));
#21208=CARTESIAN_POINT('Ctrl Pts',(-10.923590324108,34.2419663837872,-1.97108458242009));
#21209=CARTESIAN_POINT('',(-9.9959446603606,71.2419663837872,-4.82608437006737));
#21210=CARTESIAN_POINT('',(-9.99594466036059,52.7419663837872,-4.82608437006737));
#21211=CARTESIAN_POINT('',(-10.923590324108,71.2419663837872,-1.97108458242009));
#21212=CARTESIAN_POINT('Ctrl Pts',(-10.923590324108,71.2419663837872,-1.97108458242009));
#21213=CARTESIAN_POINT('Ctrl Pts',(-10.923590324108,71.4504917689707,-1.97108458242009));
#21214=CARTESIAN_POINT('Ctrl Pts',(-10.9189529481978,71.6728033656156,-1.99756320251462));
#21215=CARTESIAN_POINT('Ctrl Pts',(-10.9000247486206,72.0047784777124,-2.09788017121028));
#21216=CARTESIAN_POINT('Ctrl Pts',(-10.8893164006632,72.1320608146012,-2.15385498072772));
#21217=CARTESIAN_POINT('Ctrl Pts',(-10.8592322762978,72.345327367031,-2.30043666675911));
#21218=CARTESIAN_POINT('Ctrl Pts',(-10.8416143537529,72.4299633960731,-2.38317559106369));
#21219=CARTESIAN_POINT('Ctrl Pts',(-10.7939140781139,72.5776598312475,-2.59116419001395));
#21220=CARTESIAN_POINT('Ctrl Pts',(-10.764009678934,72.6320095746662,-2.7135485107171));
#21221=CARTESIAN_POINT('Ctrl Pts',(-10.7042980072763,72.6993182274866,-2.93911687054849));
#21222=CARTESIAN_POINT('Ctrl Pts',(-10.6757052794772,72.719076949585,-3.04144651236021));
#21223=CARTESIAN_POINT('Ctrl Pts',(-10.6303993749193,72.7379457354566,-3.19493493602834));
#21224=CARTESIAN_POINT('Ctrl Pts',(-10.6143607632876,72.7425013416222,-3.24782679425093));
#21225=CARTESIAN_POINT('Ctrl Pts',(-10.5848352611148,72.7475581223538,-3.34263644013226));
#21226=CARTESIAN_POINT('Ctrl Pts',(-10.571371962778,72.7486976181121,-3.38497499426931));
#21227=CARTESIAN_POINT('Ctrl Pts',(-10.5440464900604,72.7488007243628,-3.46915541003349));
#21228=CARTESIAN_POINT('Ctrl Pts',(-10.5300948669953,72.7477675826252,-3.51127515430947));
#21229=CARTESIAN_POINT('Ctrl Pts',(-10.4986577588269,72.7430091857572,-3.60431760807713));
#21230=CARTESIAN_POINT('Ctrl Pts',(-10.4809238053836,72.7387110754265,-3.65556102000506));
#21231=CARTESIAN_POINT('Ctrl Pts',(-10.42778755542,72.7206077607172,-3.80556850694213));
#21232=CARTESIAN_POINT('Ctrl Pts',(-10.3907943608645,72.7013249659841,-3.90536089275047));
#21233=CARTESIAN_POINT('Ctrl Pts',(-10.3076569309066,72.6362267971511,-4.12052228122571));
#21234=CARTESIAN_POINT('Ctrl Pts',(-10.2609194762829,72.5843799091732,-4.23508469600187));
#21235=CARTESIAN_POINT('Ctrl Pts',(-10.177385128307,72.4419884523094,-4.43185171084982));
#21236=CARTESIAN_POINT('Ctrl Pts',(-10.1423018038739,72.3586087195709,-4.51097817587566));
#21237=CARTESIAN_POINT('Ctrl Pts',(-10.0795534681954,72.1488438578611,-4.64962390940142));
#21238=CARTESIAN_POINT('Ctrl Pts',(-10.0549181365495,72.0245694303458,-4.70216603154109));
#21239=CARTESIAN_POINT('Ctrl Pts',(-10.0078136462567,71.6831286857266,-4.80191260915753));
#21240=CARTESIAN_POINT('Ctrl Pts',(-9.99594466036059,71.4507884295542,-4.82608437006737));
#21241=CARTESIAN_POINT('Ctrl Pts',(-9.99594466036059,71.2419663837872,-4.82608437006737));
#21242=CARTESIAN_POINT('',(-10.923590324108,52.7419663837872,-1.97108458242009));
#21243=CARTESIAN_POINT('',(-7.67879576322568,34.2419663837872,8.01536621912358));
#21244=CARTESIAN_POINT('',(-5.25018788601862,34.2419663837872,9.77985312576336));
#21245=CARTESIAN_POINT('Ctrl Pts',(-7.67879576322567,34.2419663837872,8.01536621912358));
#21246=CARTESIAN_POINT('Ctrl Pts',(-7.67879576322567,34.0448673617029,8.01536621912358));
#21247=CARTESIAN_POINT('Ctrl Pts',(-7.66152684554398,33.8362237308833,8.03205648684773));
#21248=CARTESIAN_POINT('Ctrl Pts',(-7.59418033801888,33.5102351295641,8.09567240932681));
#21249=CARTESIAN_POINT('Ctrl Pts',(-7.55382602887025,33.3781157666079,8.13362604354948));
#21250=CARTESIAN_POINT('Ctrl Pts',(-7.44618711609206,33.1591718022946,8.23218366230037));
#21251=CARTESIAN_POINT('Ctrl Pts',(-7.38548192092003,33.0725369802665,8.28699571112944));
#21252=CARTESIAN_POINT('Ctrl Pts',(-7.22536803789698,32.9165975969898,8.42716993540006));
#21253=CARTESIAN_POINT('Ctrl Pts',(-7.12688810753166,32.8583610724962,8.51092762894583));
#21254=CARTESIAN_POINT('Ctrl Pts',(-6.93933138356723,32.7862330357378,8.66412193177461));
#21255=CARTESIAN_POINT('Ctrl Pts',(-6.85215644359495,32.7652602373855,8.73327395515536));
#21256=CARTESIAN_POINT('Ctrl Pts',(-6.72152652835995,32.7459057253595,8.83368945711258));
#21257=CARTESIAN_POINT('Ctrl Pts',(-6.6775483142271,32.741377542263,8.86698199156256));
#21258=CARTESIAN_POINT('Ctrl Pts',(-6.5980244831879,32.7363522396233,8.92625499282794));
#21259=CARTESIAN_POINT('Ctrl Pts',(-6.56225065153487,32.7352238081385,8.95258770528945));
#21260=CARTESIAN_POINT('Ctrl Pts',(-6.49066230743893,32.7351419995549,9.00462430852795));
#21261=CARTESIAN_POINT('Ctrl Pts',(-6.45461199524146,32.7361860749744,9.03050029321104));
#21262=CARTESIAN_POINT('Ctrl Pts',(-6.37439764578071,32.7409747471531,9.08735308269973));
#21263=CARTESIAN_POINT('Ctrl Pts',(-6.32984230970417,32.7452987075796,9.11844270944687));
#21264=CARTESIAN_POINT('Ctrl Pts',(-6.19815827339437,32.7635405469734,9.20891143128421));
#21265=CARTESIAN_POINT('Ctrl Pts',(-6.10911631123291,32.7830083481295,9.26818457797555));
#21266=CARTESIAN_POINT('Ctrl Pts',(-5.91429278588986,32.8488643339235,9.39403227035053));
#21267=CARTESIAN_POINT('Ctrl Pts',(-5.8085865228086,32.901395231358,9.45953584447143));
#21268=CARTESIAN_POINT('Ctrl Pts',(-5.62539455535209,33.0452362980266,9.56949920370674));
#21269=CARTESIAN_POINT('Ctrl Pts',(-5.55096316769673,33.1289571391803,9.61259279303143));
#21270=CARTESIAN_POINT('Ctrl Pts',(-5.41930361233409,33.339666956537,9.6874930593962));
#21271=CARTESIAN_POINT('Ctrl Pts',(-5.36873354990731,33.4647551607023,9.71537006893975));
#21272=CARTESIAN_POINT('Ctrl Pts',(-5.27515935056375,33.7994478579448,9.76662451478779));
#21273=CARTESIAN_POINT('Ctrl Pts',(-5.25018788601862,34.0281657983111,9.77985312576336));
#21274=CARTESIAN_POINT('Ctrl Pts',(-5.25018788601862,34.2419663837872,9.77985312576336));
#21275=CARTESIAN_POINT('',(-7.67879576322568,71.2419663837872,8.01536621912358));
#21276=CARTESIAN_POINT('',(-7.67879576322568,52.7419663837872,8.01536621912358));
#21277=CARTESIAN_POINT('',(-5.25018788601862,71.2419663837872,9.77985312576336));
#21278=CARTESIAN_POINT('Ctrl Pts',(-5.25018788601862,71.2419663837872,9.77985312576336));
#21279=CARTESIAN_POINT('Ctrl Pts',(-5.25018788601862,71.4504917689704,9.77985312576336));
#21280=CARTESIAN_POINT('Ctrl Pts',(-5.27393752223651,71.6728033656151,9.76726037558861));
#21281=CARTESIAN_POINT('Ctrl Pts',(-5.36349549366727,72.0047784777118,9.71825893988788));
#21282=CARTESIAN_POINT('Ctrl Pts',(-5.41342163950681,72.1320608146007,9.69077752838638));
#21283=CARTESIAN_POINT('Ctrl Pts',(-5.54353260148699,72.3453273670309,9.61686959382355));
#21284=CARTESIAN_POINT('Ctrl Pts',(-5.61677775712631,72.4299633960731,9.57454622007711));
#21285=CARTESIAN_POINT('Ctrl Pts',(-5.79984647366443,72.5776598312476,9.46490855038957));
#21286=CARTESIAN_POINT('Ctrl Pts',(-5.90699991180841,72.6320095746663,9.39864894174127));
#21287=CARTESIAN_POINT('Ctrl Pts',(-6.10307624899109,72.6993182274867,9.27215531073132));
#21288=CARTESIAN_POINT('Ctrl Pts',(-6.19156188284057,72.719076949585,9.21334041229131));
#21289=CARTESIAN_POINT('Ctrl Pts',(-6.32353775389205,72.7379457354567,9.12282140518168));
#21290=CARTESIAN_POINT('Ctrl Pts',(-6.36888469675312,72.7425013416222,9.09122329602228));
#21291=CARTESIAN_POINT('Ctrl Pts',(-6.44993014633738,72.7475581223538,9.0338450829759));
#21292=CARTESIAN_POINT('Ctrl Pts',(-6.48603611615359,72.7486976181121,9.00795739261613));
#21293=CARTESIAN_POINT('Ctrl Pts',(-6.557652413661,72.7488007243628,8.95595614466297));
#21294=CARTESIAN_POINT('Ctrl Pts',(-6.59339938229302,72.7477675826252,8.9296716458541));
#21295=CARTESIAN_POINT('Ctrl Pts',(-6.67217341356312,72.7430091857572,8.87102147986425));
#21296=CARTESIAN_POINT('Ctrl Pts',(-6.71542870140254,72.7387110754264,8.83832040274711));
#21297=CARTESIAN_POINT('Ctrl Pts',(-6.8416742950901,72.7206077607173,8.74142996322145));
#21298=CARTESIAN_POINT('Ctrl Pts',(-6.92515096809606,72.7013249659843,8.67540980135677));
#21299=CARTESIAN_POINT('Ctrl Pts',(-7.10409072993496,72.6362267971512,8.52985288127507));
#21300=CARTESIAN_POINT('Ctrl Pts',(-7.19860339327767,72.5843799091734,8.45000118741782));
#21301=CARTESIAN_POINT('Ctrl Pts',(-7.35992641180236,72.4419884523097,8.3097509499203));
#21302=CARTESIAN_POINT('Ctrl Pts',(-7.42433880850778,72.358608719571,8.25193330320691));
#21303=CARTESIAN_POINT('Ctrl Pts',(-7.53680843474087,72.148843857861,8.14941220181591));
#21304=CARTESIAN_POINT('Ctrl Pts',(-7.57916622624129,72.0245694303456,8.1097462004612));
#21305=CARTESIAN_POINT('Ctrl Pts',(-7.65947477084994,71.6831286857259,8.03412378040701));
#21306=CARTESIAN_POINT('Ctrl Pts',(-7.67879576322567,71.4507884295537,8.01536621912358));
#21307=CARTESIAN_POINT('Ctrl Pts',(-7.67879576322567,71.2419663837872,8.01536621912358));
#21308=CARTESIAN_POINT('',(-5.25018788601862,52.7419663837872,9.77985312576336));
#21309=CARTESIAN_POINT('',(5.25018788601848,34.2419663837872,9.77985312576343));
#21310=CARTESIAN_POINT('',(7.67879576322556,34.2419663837872,8.01536621912369));
#21311=CARTESIAN_POINT('Ctrl Pts',(5.25018788601849,34.2419663837872,9.77985312576343));
#21312=CARTESIAN_POINT('Ctrl Pts',(5.25018788601848,34.0448673617023,9.77985312576343));
#21313=CARTESIAN_POINT('Ctrl Pts',(5.27139766293454,33.8362237308821,9.76858698544023));
#21314=CARTESIAN_POINT('Ctrl Pts',(5.35271121588598,33.5102351295624,9.72419505176733));
#21315=CARTESIAN_POINT('Ctrl Pts',(5.40127743435387,33.3781157666064,9.69754414106393));
#21316=CARTESIAN_POINT('Ctrl Pts',(5.5282735532022,33.1591718022934,9.6256294307783));
#21317=CARTESIAN_POINT('Ctrl Pts',(5.59916184636776,33.0725369802654,9.58483321392157));
#21318=CARTESIAN_POINT('Ctrl Pts',(5.78195336666647,32.9165975969892,9.47587207959607));
#21319=CARTESIAN_POINT('Ctrl Pts',(5.89204363899056,32.8583610724958,9.40809465081323));
#21320=CARTESIAN_POINT('Ctrl Pts',(6.09569829406898,32.7862330357376,9.27705724932768));
#21321=CARTESIAN_POINT('Ctrl Pts',(6.18840431445511,32.7652602373854,9.21551810502958));
#21322=CARTESIAN_POINT('Ctrl Pts',(6.32427199570975,32.7459057253595,9.12231176952585));
#21323=CARTESIAN_POINT('Ctrl Pts',(6.36952509309167,32.741377542263,9.09077396133064));
#21324=CARTESIAN_POINT('Ctrl Pts',(6.45047128243415,32.7363522396234,9.03345866831884));
#21325=CARTESIAN_POINT('Ctrl Pts',(6.48656990214692,32.7352238081385,9.00757298827111));
#21326=CARTESIAN_POINT('Ctrl Pts',(6.55818166766807,32.7351419995549,8.95556862185776));
#21327=CARTESIAN_POINT('Ctrl Pts',(6.59393135063794,32.7361860749744,8.92927885654121));
#21328=CARTESIAN_POINT('Ctrl Pts',(6.67278916372664,32.7409747471532,8.87055895491594));
#21329=CARTESIAN_POINT('Ctrl Pts',(6.71612551187153,32.7452987075796,8.83779153521818));
#21330=CARTESIAN_POINT('Ctrl Pts',(6.8428589844036,32.7635405469734,8.74050894690068));
#21331=CARTESIAN_POINT('Ctrl Pts',(6.92674657632628,32.7830083481296,8.67414141820088));
#21332=CARTESIAN_POINT('Ctrl Pts',(7.10663862445558,32.8488643339238,8.52774231054223));
#21333=CARTESIAN_POINT('Ctrl Pts',(7.20160125716803,32.9013952313585,8.44745139782109));
#21334=CARTESIAN_POINT('Ctrl Pts',(7.36279205769948,33.0452362980275,8.30720603020091));
#21335=CARTESIAN_POINT('Ctrl Pts',(7.42677706033756,33.1289571391813,8.24973422540444));
#21336=CARTESIAN_POINT('Ctrl Pts',(7.5386964868147,33.3396669565382,8.14766400253439));
#21337=CARTESIAN_POINT('Ctrl Pts',(7.58083610709228,33.4647551607036,8.10818348483534));
#21338=CARTESIAN_POINT('Ctrl Pts',(7.65849799963697,33.7994478579458,8.03502762759721));
#21339=CARTESIAN_POINT('Ctrl Pts',(7.67879576322556,34.0281657983116,8.01536621912369));
#21340=CARTESIAN_POINT('Ctrl Pts',(7.67879576322556,34.2419663837872,8.01536621912369));
#21341=CARTESIAN_POINT('',(5.25018788601848,71.2419663837872,9.77985312576343));
#21342=CARTESIAN_POINT('',(5.25018788601848,52.7419663837872,9.77985312576343));
#21343=CARTESIAN_POINT('',(7.67879576322556,71.2419663837872,8.01536621912369));
#21344=CARTESIAN_POINT('Ctrl Pts',(7.67879576322556,71.2419663837872,8.01536621912369));
#21345=CARTESIAN_POINT('Ctrl Pts',(7.67879576322556,71.4504917689703,8.01536621912369));
#21346=CARTESIAN_POINT('Ctrl Pts',(7.65948030491229,71.6728033656148,8.03406209159839));
#21347=CARTESIAN_POINT('Ctrl Pts',(7.58520223502748,72.0047784777117,8.10409450753346));
#21348=CARTESIAN_POINT('Ctrl Pts',(7.54363783201395,72.1320608146005,8.14308487068425));
#21349=CARTESIAN_POINT('Ctrl Pts',(7.43314071083581,72.3453273670306,8.24398894111778));
#21350=CARTESIAN_POINT('Ctrl Pts',(7.37025479259449,72.4299633960729,8.30057058192867));
#21351=CARTESIAN_POINT('Ctrl Pts',(7.20941182785805,72.5776598312474,8.44079937456493));
#21352=CARTESIAN_POINT('Ctrl Pts',(7.1132829618938,72.6320095746662,8.52223300504219));
#21353=CARTESIAN_POINT('Ctrl Pts',(6.93238944946754,72.6993182274866,8.66962400154893));
#21354=CARTESIAN_POINT('Ctrl Pts',(6.84910959243338,72.719076949585,8.7356040370796));
#21355=CARTESIAN_POINT('Ctrl Pts',(6.72223811387084,72.7379457354567,8.83314863772604));
#21356=CARTESIAN_POINT('Ctrl Pts',(6.67817355026518,72.7425013416222,8.86651179050775));
#21357=CARTESIAN_POINT('Ctrl Pts',(6.59855920561551,72.7475581223538,8.92585975051291));
#21358=CARTESIAN_POINT('Ctrl Pts',(6.56278119073521,72.7486976181121,8.95219883211764));
#21359=CARTESIAN_POINT('Ctrl Pts',(6.49119441200987,72.7488007243628,9.00424070918876));
#21360=CARTESIAN_POINT('Ctrl Pts',(6.45514994733567,72.7477675826252,9.03011573982332));
#21361=CARTESIAN_POINT('Ctrl Pts',(6.37502781041205,72.7430091857572,9.08691039756332));
#21362=CARTESIAN_POINT('Ctrl Pts',(6.33056061889071,72.7387110754265,9.11794343236385));
#21363=CARTESIAN_POINT('Ctrl Pts',(6.19940030109836,72.7206077607173,9.20806933448832));
#21364=CARTESIAN_POINT('Ctrl Pts',(6.11081568535757,72.7013249659843,9.26705901632157));
#21365=CARTESIAN_POINT('Ctrl Pts',(5.91708740064485,72.6362267971514,9.39226128088835));
#21366=CARTESIAN_POINT('Ctrl Pts',(5.81193790770809,72.5843799091737,9.45747263480139));
#21367=CARTESIAN_POINT('Ctrl Pts',(5.62870045111611,72.44198845231,9.56756023594587));
#21368=CARTESIAN_POINT('Ctrl Pts',(5.55380807622207,72.3586087195714,9.61095343015356));
#21369=CARTESIAN_POINT('Ctrl Pts',(5.42154968882926,72.1488438578613,9.68623763845605));
#21370=CARTESIAN_POINT('Ctrl Pts',(5.37073580234758,72.0245694303458,9.71426482356093));
#21371=CARTESIAN_POINT('Ctrl Pts',(5.27399790189939,71.6831286857264,9.7672741752727));
#21372=CARTESIAN_POINT('Ctrl Pts',(5.25018788601848,71.4507884295543,9.77985312576343));
#21373=CARTESIAN_POINT('Ctrl Pts',(5.25018788601848,71.2419663837872,9.77985312576343));
#21374=CARTESIAN_POINT('',(7.67879576322556,52.7419663837872,8.01536621912369));
#21375=CARTESIAN_POINT('',(10.923590324108,34.2419663837872,-1.97108458241993));
#21376=CARTESIAN_POINT('',(9.99594466036066,34.2419663837872,-4.82608437006722));
#21377=CARTESIAN_POINT('Ctrl Pts',(10.923590324108,34.2419663837872,-1.97108458241994));
#21378=CARTESIAN_POINT('Ctrl Pts',(10.923590324108,34.0448673617023,-1.97108458241993));
#21379=CARTESIAN_POINT('Ctrl Pts',(10.9194297694541,33.836223730882,-1.99473770778586));
#21380=CARTESIAN_POINT('Ctrl Pts',(10.9023378013986,33.5102351295626,-2.08578935410117));
#21381=CARTESIAN_POINT('Ctrl Pts',(10.8919990659681,33.3781157666067,-2.14021415696957));
#21382=CARTESIAN_POINT('Ctrl Pts',(10.8628480710774,33.1591718022937,-2.28321751096788));
#21383=CARTESIAN_POINT('Ctrl Pts',(10.8459542504861,33.0725369802659,-2.36324300842669));
#21384=CARTESIAN_POINT('Ctrl Pts',(10.7988117398629,32.9165975969896,-2.57075891716293));
#21385=CARTESIAN_POINT('Ctrl Pts',(10.7683713396248,32.8583610724961,-2.69640536536647));
#21386=CARTESIAN_POINT('Ctrl Pts',(10.7066801144663,32.7862330357377,-2.93058523611078));
#21387=CARTESIAN_POINT('Ctrl Pts',(10.6768006460545,32.7652602373855,-3.03777054230638));
#21388=CARTESIAN_POINT('Ctrl Pts',(10.6301415758076,32.7459057253595,-3.1957907275721));
#21389=CARTESIAN_POINT('Ctrl Pts',(10.6141313139529,32.741377542263,-3.24857469941767));
#21390=CARTESIAN_POINT('Ctrl Pts',(10.5846349791874,32.7363522396234,-3.34327049983937));
#21391=CARTESIAN_POINT('Ctrl Pts',(10.5711713214639,32.7352238081385,-3.38560144239239));
#21392=CARTESIAN_POINT('Ctrl Pts',(10.5438414824539,32.7351419995549,-3.46977851163795));
#21393=CARTESIAN_POINT('Ctrl Pts',(10.5298856894189,32.7361860749744,-3.51190246484306));
#21394=CARTESIAN_POINT('Ctrl Pts',(10.4984081487255,32.7409747471532,-3.60504614935238));
#21395=CARTESIAN_POINT('Ctrl Pts',(10.4806361487507,32.7452987075796,-3.65638715519652));
#21396=CARTESIAN_POINT('Ctrl Pts',(10.4272777059778,32.7635405469734,-3.80697982312781));
#21397=CARTESIAN_POINT('Ctrl Pts',(10.3900811268587,32.7830083481296,-3.90727035830519));
#21398=CARTESIAN_POINT('Ctrl Pts',(10.306437001565,32.8488643339237,-4.12359767513608));
#21399=CARTESIAN_POINT('Ctrl Pts',(10.259420873161,32.9013952313583,-4.23872376230644));
#21400=CARTESIAN_POINT('Ctrl Pts',(10.1758502991068,33.0452362980271,-4.43536352549553));
#21401=CARTESIAN_POINT('Ctrl Pts',(10.1409638178522,33.1289571391808,-4.51397664357904));
#21402=CARTESIAN_POINT('Ctrl Pts',(10.0784742720542,33.3396669565371,-4.65195977691635));
#21403=CARTESIAN_POINT('Ctrl Pts',(10.0539479272322,33.4647551607021,-4.70423708829116));
#21404=CARTESIAN_POINT('Ctrl Pts',(10.0083714171123,33.7994478579445,-4.8007043403884));
#21405=CARTESIAN_POINT('Ctrl Pts',(9.99594466036066,34.028165798311,-4.82608437006722));
#21406=CARTESIAN_POINT('Ctrl Pts',(9.99594466036066,34.2419663837872,-4.82608437006722));
#21407=CARTESIAN_POINT('',(10.923590324108,71.2419663837872,-1.97108458241994));
#21408=CARTESIAN_POINT('',(10.923590324108,52.7419663837872,-1.97108458241993));
#21409=CARTESIAN_POINT('',(9.99594466036066,71.2419663837872,-4.82608437006722));
#21410=CARTESIAN_POINT('Ctrl Pts',(9.99594466036066,71.2419663837872,-4.82608437006722));
#21411=CARTESIAN_POINT('Ctrl Pts',(9.99594466036066,71.4504917689704,-4.82608437006722));
#21412=CARTESIAN_POINT('Ctrl Pts',(10.0077566868326,71.6728033656151,-4.8019369352539));
#21413=CARTESIAN_POINT('Ctrl Pts',(10.0514082864556,72.0047784777116,-4.70965308619137));
#21414=CARTESIAN_POINT('Ctrl Pts',(10.0756462185105,72.1320608146004,-4.65807430502919));
#21415=CARTESIAN_POINT('Ctrl Pts',(10.1374662039433,72.3453273670303,-4.52180422533572));
#21416=CARTESIAN_POINT('Ctrl Pts',(10.1718457246956,72.4299633960724,-4.44451147442918));
#21417=CARTESIAN_POINT('Ctrl Pts',(10.2555080221753,72.5776598312471,-4.24820764469131));
#21418=CARTESIAN_POINT('Ctrl Pts',(10.3032505538534,72.632009574666,-4.13161928458072));
#21419=CARTESIAN_POINT('Ctrl Pts',(10.3875285520126,72.6993182274866,-3.91403300809339));
#21420=CARTESIAN_POINT('Ctrl Pts',(10.4245444036369,72.719076949585,-3.81444020511614));
#21421=CARTESIAN_POINT('Ctrl Pts',(10.4781093887338,72.7379457354566,-3.66363531938793));
#21422=CARTESIAN_POINT('Ctrl Pts',(10.4962229335872,72.7425013416222,-3.61141764783749));
#21423=CARTESIAN_POINT('Ctrl Pts',(10.5280640121862,72.7475581223538,-3.51736037834474));
#21424=CARTESIAN_POINT('Ctrl Pts',(10.5420579527565,72.7486976181121,-3.47519424032078));
#21425=CARTESIAN_POINT('Ctrl Pts',(10.5694311878667,72.7488007243628,-3.39102934349887));
#21426=CARTESIAN_POINT('Ctrl Pts',(10.5829014522237,72.7477675826252,-3.34875319629781));
#21427=CARTESIAN_POINT('Ctrl Pts',(10.612157279623,72.7430091857572,-3.25500200144585));
#21428=CARTESIAN_POINT('Ctrl Pts',(10.6279303317183,72.7387110754265,-3.20312145404741));
#21429=CARTESIAN_POINT('Ctrl Pts',(10.6731143910355,72.7206077607173,-3.05053014374117));
#21430=CARTESIAN_POINT('Ctrl Pts',(10.7018427606331,72.7013249659842,-2.94805235351826));
#21431=CARTESIAN_POINT('Ctrl Pts',(10.7610518579369,72.6362267971514,-2.7251161784661));
#21432=CARTESIAN_POINT('Ctrl Pts',(10.7905785607449,72.5843799091737,-2.6049616514383));
#21433=CARTESIAN_POINT('Ctrl Pts',(10.8386546030836,72.4419884523103,-2.39667353469379));
#21434=CARTESIAN_POINT('Ctrl Pts',(10.8567809666063,72.3586087195719,-2.31203741907974));
#21435=CARTESIAN_POINT('Ctrl Pts',(10.8875104141335,72.1488438578622,-2.16298811814181));
#21436=CARTESIAN_POINT('Ctrl Pts',(10.8984634966878,72.024569430347,-2.10600036378336));
#21437=CARTESIAN_POINT('Ctrl Pts',(10.9189847308192,71.6831286857275,-1.99761636264956));
#21438=CARTESIAN_POINT('Ctrl Pts',(10.923590324108,71.4507884295547,-1.97108458241993));
#21439=CARTESIAN_POINT('Ctrl Pts',(10.923590324108,71.2419663837872,-1.97108458241993));
#21440=CARTESIAN_POINT('',(9.99594466036066,52.7419663837872,-4.82608437006722));
#21441=CARTESIAN_POINT('',(1.5009622134597,34.2419663837872,-10.9980503923998));
#21442=CARTESIAN_POINT('',(-1.5009622134597,34.2419663837872,-10.9980503923998));
#21443=CARTESIAN_POINT('Ctrl Pts',(1.5009622134597,34.2419663837872,-10.9980503923998));
#21444=CARTESIAN_POINT('Ctrl Pts',(1.5009622134597,34.0448673617028,-10.9980503923998));
#21445=CARTESIAN_POINT('Ctrl Pts',(1.4771810723556,33.8362237308832,-11.001402687493));
#21446=CARTESIAN_POINT('Ctrl Pts',(1.38530410221158,33.5102351295638,-11.0132837659748));
#21447=CARTESIAN_POINT('Ctrl Pts',(1.33034819384697,33.3781157666076,-11.0202692332752));
#21448=CARTESIAN_POINT('Ctrl Pts',(1.18533576935023,33.1591718022941,-11.036735456266));
#21449=CARTESIAN_POINT('Ctrl Pts',(1.10400652085938,33.0725369802661,-11.0453977168056));
#21450=CARTESIAN_POINT('Ctrl Pts',(0.892079326680434,32.9165975969895,-11.0646884672856));
#21451=CARTESIAN_POINT('Ctrl Pts',(0.763175852377868,32.858361072496,-11.0745648140582));
#21452=CARTESIAN_POINT('Ctrl Pts',(0.521393923343685,32.7862330357377,-11.0882585321735));
#21453=CARTESIAN_POINT('Ctrl Pts',(0.410221375913344,32.7652602373854,-11.0929635501988));
#21454=CARTESIAN_POINT('Ctrl Pts',(0.245516803362354,32.7459057253595,-11.0974190600975));
#21455=CARTESIAN_POINT('Ctrl Pts',(0.190368819985358,32.741377542263,-11.0985035405639));
#21456=CARTESIAN_POINT('Ctrl Pts',(0.0911928932145149,32.7363522396234,
-11.0997134708045));
#21457=CARTESIAN_POINT('Ctrl Pts',(0.0467732754157406,32.7352238081385,
-11.0999897520302));
#21458=CARTESIAN_POINT('Ctrl Pts',(-0.0417292595203717,32.7351419995549,
-11.1000096754841));
#21459=CARTESIAN_POINT('Ctrl Pts',(-0.0861040969257631,32.7361860749744,
-11.0997539449887));
#21460=CARTESIAN_POINT('Ctrl Pts',(-0.184416100045005,32.7409747471531,
-11.0986000062274));
#21461=CARTESIAN_POINT('Ctrl Pts',(-0.238736148222333,32.7452987075796,
-11.0975630731579));
#21462=CARTESIAN_POINT('Ctrl Pts',(-0.398446951974606,32.7635405469734,
-11.0933518720784));
#21463=CARTESIAN_POINT('Ctrl Pts',(-0.505323294057916,32.7830083481295,
-11.0889673028681));
#21464=CARTESIAN_POINT('Ctrl Pts',(-0.736910254577724,32.8488643339236,
-11.0762658297061));
#21465=CARTESIAN_POINT('Ctrl Pts',(-0.860930452663105,32.9013952313582,
-11.0671267518481));
#21466=CARTESIAN_POINT('Ctrl Pts',(-1.07377070841952,33.0452362980269,-11.0484114414186));
#21467=CARTESIAN_POINT('Ctrl Pts',(-1.15931674222102,33.1289571391807,-11.0395252155594));
#21468=CARTESIAN_POINT('Ctrl Pts',(-1.30985683194327,33.3396669565376,-11.0227332589661));
#21469=CARTESIAN_POINT('Ctrl Pts',(-1.36715456694085,33.464755160703,-11.0155618965373));
#21470=CARTESIAN_POINT('Ctrl Pts',(-1.47298429182855,33.7994478579454,-11.0020260798964));
#21471=CARTESIAN_POINT('Ctrl Pts',(-1.5009622134597,34.0281657983114,-10.9980503923998));
#21472=CARTESIAN_POINT('Ctrl Pts',(-1.5009622134597,34.2419663837872,-10.9980503923998));
#21473=CARTESIAN_POINT('',(1.5009622134597,71.2419663837872,-10.9980503923998));
#21474=CARTESIAN_POINT('',(1.5009622134597,52.7419663837872,-10.9980503923998));
#21475=CARTESIAN_POINT('',(-1.5009622134597,71.2419663837872,-10.9980503923998));
#21476=CARTESIAN_POINT('Ctrl Pts',(-1.5009622134597,71.2419663837872,-10.9980503923998));
#21477=CARTESIAN_POINT('Ctrl Pts',(-1.5009622134597,71.4504917689704,-10.9980503923998));
#21478=CARTESIAN_POINT('Ctrl Pts',(-1.47434652131067,71.672803365615,-11.0018223294187));
#21479=CARTESIAN_POINT('Ctrl Pts',(-1.37309027919532,72.0047784777118,-11.0148201900203));
#21480=CARTESIAN_POINT('Ctrl Pts',(-1.31654601035469,72.1320608146007,-11.0219331133145));
#21481=CARTESIAN_POINT('Ctrl Pts',(-1.1678420369948,72.3453273670308,-11.0386176428475));
#21482=CARTESIAN_POINT('Ctrl Pts',(-1.08370840641146,72.4299633960732,-11.0474297365141));
#21483=CARTESIAN_POINT('Ctrl Pts',(-0.871159298255557,72.5776598312476,
-11.0663360902504));
#21484=CARTESIAN_POINT('Ctrl Pts',(-0.745523925005287,72.6320095746663,
-11.0757141514867));
#21485=CARTESIAN_POINT('Ctrl Pts',(-0.512543745213127,72.6993182274867,
-11.088629433639));
#21486=CARTESIAN_POINT('Ctrl Pts',(-0.40638683375279,72.7190769495851,-11.0930577318951));
#21487=CARTESIAN_POINT('Ctrl Pts',(-0.246410373793683,72.7379457354567,
-11.0973997874919));
#21488=CARTESIAN_POINT('Ctrl Pts',(-0.191151023812067,72.7425013416222,
-11.0984906444421));
#21489=CARTESIAN_POINT('Ctrl Pts',(-0.0918578103498296,72.7475581223538,
-11.0997080150118));
#21490=CARTESIAN_POINT('Ctrl Pts',(-0.047431064560685,72.7486976181121,
-11.0999869901433));
#21491=CARTESIAN_POINT('Ctrl Pts',(0.0410733038449227,72.7488007243628,
-11.1000121003192));
#21492=CARTESIAN_POINT('Ctrl Pts',(0.0854428497291022,72.7477675826252,
-11.0997590350702));
#21493=CARTESIAN_POINT('Ctrl Pts',(0.183646082354475,72.7430091857572,-11.0986122679057));
#21494=CARTESIAN_POINT('Ctrl Pts',(0.237861556176987,72.7387110754265,-11.0975813610593));
#21495=CARTESIAN_POINT('Ctrl Pts',(0.396947158376942,72.7206077607173,-11.093400647027));
#21496=CARTESIAN_POINT('Ctrl Pts',(0.503286882970486,72.7013249659843,-11.0890555714104));
#21497=CARTESIAN_POINT('Ctrl Pts',(0.733608402260471,72.6362267971513,-11.0764757024731));
#21498=CARTESIAN_POINT('Ctrl Pts',(0.857006401108316,72.5843799091735,-11.0674274747807));
#21499=CARTESIAN_POINT('Ctrl Pts',(1.0699564859103,72.4419884523097,-11.0487859403242));
#21500=CARTESIAN_POINT('Ctrl Pts',(1.15605156955383,72.358608719571,-11.0398711384066));
#21501=CARTESIAN_POINT('Ctrl Pts',(1.30730179997395,72.1488438578608,-11.0230378127299));
#21502=CARTESIAN_POINT('Ctrl Pts',(1.36488506375574,72.0245694303452,-11.0158446286986));
#21503=CARTESIAN_POINT('Ctrl Pts',(1.47430578438809,71.6831286857259,-11.0018689838731));
#21504=CARTESIAN_POINT('Ctrl Pts',(1.5009622134597,71.4507884295539,-10.9980503923998));
#21505=CARTESIAN_POINT('Ctrl Pts',(1.5009622134597,71.2419663837872,-10.9980503923998));
#21506=CARTESIAN_POINT('',(-1.5009622134597,52.7419663837872,-10.9980503923998));
#21507=CARTESIAN_POINT('',(7.67879576322562,34.2419663837872,-8.01536621912364));
#21508=CARTESIAN_POINT('',(5.25018788601855,34.2419663837872,-9.7798531257634));
#21509=CARTESIAN_POINT('Ctrl Pts',(7.67879576322562,34.2419663837872,-8.01536621912364));
#21510=CARTESIAN_POINT('Ctrl Pts',(7.67879576322562,34.0448673617025,-8.01536621912364));
#21511=CARTESIAN_POINT('Ctrl Pts',(7.66152684554386,33.8362237308826,-8.03205648684785));
#21512=CARTESIAN_POINT('Ctrl Pts',(7.59418033801855,33.5102351295631,-8.09567240932711));
#21513=CARTESIAN_POINT('Ctrl Pts',(7.55382602886988,33.3781157666071,-8.13362604354981));
#21514=CARTESIAN_POINT('Ctrl Pts',(7.44618711609161,33.1591718022939,-8.23218366230077));
#21515=CARTESIAN_POINT('Ctrl Pts',(7.38548192091953,33.072536980266,-8.2869957111299));
#21516=CARTESIAN_POINT('Ctrl Pts',(7.22536803789647,32.9165975969895,-8.42716993540051));
#21517=CARTESIAN_POINT('Ctrl Pts',(7.12688810753123,32.858361072496,-8.51092762894619));
#21518=CARTESIAN_POINT('Ctrl Pts',(6.93933138356694,32.7862330357377,-8.66412193177484));
#21519=CARTESIAN_POINT('Ctrl Pts',(6.8521564435947,32.7652602373854,-8.73327395515555));
#21520=CARTESIAN_POINT('Ctrl Pts',(6.72152652835974,32.7459057253595,-8.83368945711273));
#21521=CARTESIAN_POINT('Ctrl Pts',(6.67754831422682,32.741377542263,-8.86698199156276));
#21522=CARTESIAN_POINT('Ctrl Pts',(6.59802448318803,32.7363522396234,-8.92625499282784));
#21523=CARTESIAN_POINT('Ctrl Pts',(6.56225065153525,32.7352238081385,-8.95258770528917));
#21524=CARTESIAN_POINT('Ctrl Pts',(6.49066230743835,32.7351419995549,-9.00462430852837));
#21525=CARTESIAN_POINT('Ctrl Pts',(6.45461199524108,32.7361860749744,-9.03050029321131));
#21526=CARTESIAN_POINT('Ctrl Pts',(6.37439764578055,32.7409747471532,-9.08735308269985));
#21527=CARTESIAN_POINT('Ctrl Pts',(6.32984230970395,32.7452987075796,-9.11844270944702));
#21528=CARTESIAN_POINT('Ctrl Pts',(6.19815827339409,32.7635405469734,-9.20891143128439));
#21529=CARTESIAN_POINT('Ctrl Pts',(6.10911631123248,32.7830083481296,-9.26818457797584));
#21530=CARTESIAN_POINT('Ctrl Pts',(5.91429278588921,32.8488643339237,-9.39403227035094));
#21531=CARTESIAN_POINT('Ctrl Pts',(5.8085865228078,32.9013952313582,-9.45953584447193));
#21532=CARTESIAN_POINT('Ctrl Pts',(5.62539455535125,33.045236298027,-9.56949920370723));
#21533=CARTESIAN_POINT('Ctrl Pts',(5.55096316769597,33.1289571391809,-9.61259279303187));
#21534=CARTESIAN_POINT('Ctrl Pts',(5.41930361233357,33.3396669565375,-9.6874930593965));
#21535=CARTESIAN_POINT('Ctrl Pts',(5.36873354990689,33.4647551607027,-9.71537006893998));
#21536=CARTESIAN_POINT('Ctrl Pts',(5.27515935056357,33.7994478579451,-9.76662451478789));
#21537=CARTESIAN_POINT('Ctrl Pts',(5.25018788601855,34.0281657983112,-9.7798531257634));
#21538=CARTESIAN_POINT('Ctrl Pts',(5.25018788601855,34.2419663837872,-9.7798531257634));
#21539=CARTESIAN_POINT('',(7.67879576322562,71.2419663837872,-8.01536621912364));
#21540=CARTESIAN_POINT('',(7.67879576322562,52.7419663837872,-8.01536621912364));
#21541=CARTESIAN_POINT('',(5.25018788601855,71.2419663837872,-9.7798531257634));
#21542=CARTESIAN_POINT('Ctrl Pts',(5.25018788601855,71.2419663837872,-9.7798531257634));
#21543=CARTESIAN_POINT('Ctrl Pts',(5.25018788601855,71.4504917689702,-9.7798531257634));
#21544=CARTESIAN_POINT('Ctrl Pts',(5.27393752223632,71.6728033656147,-9.76726037558871));
#21545=CARTESIAN_POINT('Ctrl Pts',(5.36349549366685,72.0047784777112,-9.71825893988811));
#21546=CARTESIAN_POINT('Ctrl Pts',(5.4134216395063,72.1320608146002,-9.69077752838666));
#21547=CARTESIAN_POINT('Ctrl Pts',(5.54353260148639,72.3453273670305,-9.61686959382389));
#21548=CARTESIAN_POINT('Ctrl Pts',(5.61677775712566,72.4299633960727,-9.57454622007749));
#21549=CARTESIAN_POINT('Ctrl Pts',(5.79984647366373,72.5776598312473,-9.46490855038999));
#21550=CARTESIAN_POINT('Ctrl Pts',(5.90699991180771,72.6320095746661,-9.39864894174172));
#21551=CARTESIAN_POINT('Ctrl Pts',(6.10307624899076,72.6993182274866,-9.27215531073154));
#21552=CARTESIAN_POINT('Ctrl Pts',(6.19156188284038,72.719076949585,-9.21334041229143));
#21553=CARTESIAN_POINT('Ctrl Pts',(6.32353775389184,72.7379457354566,-9.12282140518183));
#21554=CARTESIAN_POINT('Ctrl Pts',(6.36888469675294,72.7425013416222,-9.09122329602241));
#21555=CARTESIAN_POINT('Ctrl Pts',(6.44993014633731,72.7475581223538,-9.03384508297595));
#21556=CARTESIAN_POINT('Ctrl Pts',(6.48603611615362,72.7486976181121,-9.00795739261611));
#21557=CARTESIAN_POINT('Ctrl Pts',(6.55765241366075,72.7488007243628,-8.95595614466315));
#21558=CARTESIAN_POINT('Ctrl Pts',(6.59339938229281,72.7477675826252,-8.92967164585425));
#21559=CARTESIAN_POINT('Ctrl Pts',(6.67217341356285,72.7430091857572,-8.87102147986445));
#21560=CARTESIAN_POINT('Ctrl Pts',(6.71542870140231,72.7387110754264,-8.83832040274729));
#21561=CARTESIAN_POINT('Ctrl Pts',(6.84167429508994,72.7206077607173,-8.74142996322158));
#21562=CARTESIAN_POINT('Ctrl Pts',(6.92515096809575,72.7013249659843,-8.67540980135703));
#21563=CARTESIAN_POINT('Ctrl Pts',(7.10409072993444,72.6362267971514,-8.52985288127551));
#21564=CARTESIAN_POINT('Ctrl Pts',(7.19860339327709,72.5843799091737,-8.45000118741832));
#21565=CARTESIAN_POINT('Ctrl Pts',(7.35992641180176,72.4419884523103,-8.30975094992083));
#21566=CARTESIAN_POINT('Ctrl Pts',(7.42433880850722,72.3586087195718,-8.2519333032074));
#21567=CARTESIAN_POINT('Ctrl Pts',(7.53680843474049,72.1488438578617,-8.14941220181626));
#21568=CARTESIAN_POINT('Ctrl Pts',(7.57916622624094,72.0245694303463,-8.10974620046152));
#21569=CARTESIAN_POINT('Ctrl Pts',(7.65947477084968,71.6831286857272,-8.03412378040726));
#21570=CARTESIAN_POINT('Ctrl Pts',(7.67879576322561,71.4507884295547,-8.01536621912364));
#21571=CARTESIAN_POINT('Ctrl Pts',(7.67879576322561,71.2419663837872,-8.01536621912364));
#21572=CARTESIAN_POINT('',(5.25018788601855,52.7419663837872,-9.7798531257634));
#21573=CARTESIAN_POINT('',(9.99594466036063,34.2419663837872,4.8260843700673));
#21574=CARTESIAN_POINT('',(10.923590324108,34.2419663837872,1.97108458242001));
#21575=CARTESIAN_POINT('Ctrl Pts',(9.99594466036063,34.2419663837872,4.82608437006729));
#21576=CARTESIAN_POINT('Ctrl Pts',(9.99594466036063,34.0448673617038,4.82608437006729));
#21577=CARTESIAN_POINT('Ctrl Pts',(10.0064816592001,33.8362237308852,4.80450307700971));
#21578=CARTESIAN_POINT('Ctrl Pts',(10.0461727814764,33.5102351295666,4.72079434102039));
#21579=CARTESIAN_POINT('Ctrl Pts',(10.0697986652976,33.3781157666103,4.67068679437128));
#21580=CARTESIAN_POINT('Ctrl Pts',(10.1302702775364,33.1591718022967,4.53786012584826));
#21581=CARTESIAN_POINT('Ctrl Pts',(10.1636406967916,33.0725369802687,4.46318819982269));
#21582=CARTESIAN_POINT('Ctrl Pts',(10.2474763953112,32.9165975969911,4.26759463055161));
#21583=CARTESIAN_POINT('Ctrl Pts',(10.2967027234602,32.858361072497,4.14805210033772));
#21584=CARTESIAN_POINT('Ctrl Pts',(10.384440948311,32.7862330357381,3.92233541281996));
#21585=CARTESIAN_POINT('Ctrl Pts',(10.4232698928273,32.7652602373856,3.81805796768124));
#21586=CARTESIAN_POINT('Ctrl Pts',(10.4784038465198,32.7459057253596,3.66279143896954));
#21587=CARTESIAN_POINT('Ctrl Pts',(10.4964769128032,32.741377542263,3.61067771291216));
#21588=CARTESIAN_POINT('Ctrl Pts',(10.528274671648,32.7363522396234,3.51672969050343));
#21589=CARTESIAN_POINT('Ctrl Pts',(10.5422638474915,32.7352238081385,3.47456949913845));
#21590=CARTESIAN_POINT('Ctrl Pts',(10.5696315831627,32.7351419995549,3.39040474326442));
#21591=CARTESIAN_POINT('Ctrl Pts',(10.5831009478896,32.7361860749744,3.34812273992123));
#21592=CARTESIAN_POINT('Ctrl Pts',(10.6123835666262,32.7409747471531,3.25426588203674));
#21593=CARTESIAN_POINT('Ctrl Pts',(10.6281832026956,32.7452987075795,3.20228401631163));
#21594=CARTESIAN_POINT('Ctrl Pts',(10.6735314650122,32.7635405469733,3.04908868298021));
#21595=CARTESIAN_POINT('Ctrl Pts',(10.7023880978939,32.7830083481293,2.94608833500536));
#21596=CARTESIAN_POINT('Ctrl Pts',(10.7618725855526,32.8488643339229,2.72191107605422));
#21597=CARTESIAN_POINT('Ctrl Pts',(10.7915051548569,32.901395231357,2.60113672814234));
#21598=CARTESIAN_POINT('Ctrl Pts',(10.8394770930343,33.0452362980247,2.39293026699778));
#21599=CARTESIAN_POINT('Ctrl Pts',(10.8574609682717,33.1289571391782,2.30882515930115));
#21600=CARTESIAN_POINT('Ctrl Pts',(10.8880103145913,33.3396669565342,2.16046402605085));
#21601=CARTESIAN_POINT('Ctrl Pts',(10.8988959174761,33.4647551606989,2.10375456894896));
#21602=CARTESIAN_POINT('Ctrl Pts',(10.918725774357,33.7994478579421,1.99892172210085));
#21603=CARTESIAN_POINT('Ctrl Pts',(10.923590324108,34.0281657983099,1.97108458242001));
#21604=CARTESIAN_POINT('Ctrl Pts',(10.923590324108,34.2419663837872,1.97108458242001));
#21605=CARTESIAN_POINT('',(9.99594466036063,71.2419663837872,4.82608437006729));
#21606=CARTESIAN_POINT('',(9.99594466036063,52.7419663837872,4.8260843700673));
#21607=CARTESIAN_POINT('',(10.923590324108,71.2419663837872,1.97108458242002));
#21608=CARTESIAN_POINT('Ctrl Pts',(10.923590324108,71.2419663837872,1.97108458242001));
#21609=CARTESIAN_POINT('Ctrl Pts',(10.923590324108,71.4504917689706,1.97108458242001));
#21610=CARTESIAN_POINT('Ctrl Pts',(10.9189529481978,71.6728033656157,1.99756320251457));
#21611=CARTESIAN_POINT('Ctrl Pts',(10.9000247486206,72.0047784777125,2.09788017121029));
#21612=CARTESIAN_POINT('Ctrl Pts',(10.8893164006632,72.1320608146013,2.15385498072775));
#21613=CARTESIAN_POINT('Ctrl Pts',(10.8592322762978,72.345327367031,2.30043666675914));
#21614=CARTESIAN_POINT('Ctrl Pts',(10.8416143537528,72.4299633960732,2.38317559106376));
#21615=CARTESIAN_POINT('Ctrl Pts',(10.7939140781138,72.5776598312476,2.59116419001411));
#21616=CARTESIAN_POINT('Ctrl Pts',(10.7640096789339,72.6320095746663,2.71354851071738));
#21617=CARTESIAN_POINT('Ctrl Pts',(10.7042980072763,72.6993182274866,2.93911687054846));
#21618=CARTESIAN_POINT('Ctrl Pts',(10.6757052794772,72.719076949585,3.04144651236001));
#21619=CARTESIAN_POINT('Ctrl Pts',(10.6303993749193,72.7379457354566,3.19493493602824));
#21620=CARTESIAN_POINT('Ctrl Pts',(10.6143607632877,72.7425013416222,3.24782679425072));
#21621=CARTESIAN_POINT('Ctrl Pts',(10.5848352611148,72.7475581223538,3.34263644013247));
#21622=CARTESIAN_POINT('Ctrl Pts',(10.5713719627778,72.7486976181121,3.38497499426978));
#21623=CARTESIAN_POINT('Ctrl Pts',(10.5440464900604,72.7488007243628,3.46915541003345));
#21624=CARTESIAN_POINT('Ctrl Pts',(10.5300948669954,72.7477675826252,3.51127515430942));
#21625=CARTESIAN_POINT('Ctrl Pts',(10.4986577588269,72.7430091857572,3.60431760807724));
#21626=CARTESIAN_POINT('Ctrl Pts',(10.4809238053836,72.7387110754264,3.65556102000509));
#21627=CARTESIAN_POINT('Ctrl Pts',(10.4277875554201,72.7206077607172,3.80556850694187));
#21628=CARTESIAN_POINT('Ctrl Pts',(10.3907943608646,72.7013249659841,3.9053608927504));
#21629=CARTESIAN_POINT('Ctrl Pts',(10.3076569309066,72.636226797151,4.12052228122582));
#21630=CARTESIAN_POINT('Ctrl Pts',(10.2609194762829,72.5843799091731,4.23508469600199));
#21631=CARTESIAN_POINT('Ctrl Pts',(10.177385128307,72.4419884523093,4.43185171084991));
#21632=CARTESIAN_POINT('Ctrl Pts',(10.1423018038739,72.3586087195708,4.51097817587572));
#21633=CARTESIAN_POINT('Ctrl Pts',(10.0795534681954,72.1488438578609,4.64962390940149));
#21634=CARTESIAN_POINT('Ctrl Pts',(10.0549181365495,72.0245694303455,4.70216603154115));
#21635=CARTESIAN_POINT('Ctrl Pts',(10.0078136462567,71.6831286857264,4.80191260915748));
#21636=CARTESIAN_POINT('Ctrl Pts',(9.99594466036063,71.4507884295541,4.8260843700673));
#21637=CARTESIAN_POINT('Ctrl Pts',(9.99594466036063,71.2419663837872,4.8260843700673));
#21638=CARTESIAN_POINT('',(10.923590324108,52.7419663837872,1.97108458242001));
#21639=CARTESIAN_POINT('',(-10.923590324108,34.2419663837872,1.97108458241986));
#21640=CARTESIAN_POINT('',(-9.99594466036069,34.2419663837872,4.82608437006716));
#21641=CARTESIAN_POINT('Ctrl Pts',(-10.923590324108,34.2419663837872,1.97108458241986));
#21642=CARTESIAN_POINT('Ctrl Pts',(-10.923590324108,34.0448673617026,1.97108458241986));
#21643=CARTESIAN_POINT('Ctrl Pts',(-10.9194297694542,33.8362237308825,1.99473770778571));
#21644=CARTESIAN_POINT('Ctrl Pts',(-10.9023378013987,33.5102351295631,2.08578935410087));
#21645=CARTESIAN_POINT('Ctrl Pts',(-10.8919990659682,33.3781157666071,2.14021415696922));
#21646=CARTESIAN_POINT('Ctrl Pts',(-10.8628480710775,33.1591718022942,2.28321751096736));
#21647=CARTESIAN_POINT('Ctrl Pts',(-10.8459542504862,33.0725369802663,2.36324300842611));
#21648=CARTESIAN_POINT('Ctrl Pts',(-10.798811739863,32.9165975969897,2.57075891716242));
#21649=CARTESIAN_POINT('Ctrl Pts',(-10.7683713396249,32.8583610724962,2.69640536536613));
#21650=CARTESIAN_POINT('Ctrl Pts',(-10.7066801144664,32.7862330357378,2.93058523611043));
#21651=CARTESIAN_POINT('Ctrl Pts',(-10.6768006460546,32.7652602373855,3.03777054230603));
#21652=CARTESIAN_POINT('Ctrl Pts',(-10.6301415758076,32.7459057253595,3.19579072757192));
#21653=CARTESIAN_POINT('Ctrl Pts',(-10.6141313139529,32.741377542263,3.24857469941753));
#21654=CARTESIAN_POINT('Ctrl Pts',(-10.5846349791873,32.7363522396233,3.34327049983945));
#21655=CARTESIAN_POINT('Ctrl Pts',(-10.5711713214638,32.7352238081385,3.3856014423927));
#21656=CARTESIAN_POINT('Ctrl Pts',(-10.5438414824541,32.7351419995549,3.46977851163747));
#21657=CARTESIAN_POINT('Ctrl Pts',(-10.529885689419,32.7361860749744,3.51190246484276));
#21658=CARTESIAN_POINT('Ctrl Pts',(-10.4984081487255,32.7409747471532,3.60504614935233));
#21659=CARTESIAN_POINT('Ctrl Pts',(-10.4806361487507,32.7452987075796,3.65638715519642));
#21660=CARTESIAN_POINT('Ctrl Pts',(-10.4272777059778,32.7635405469734,3.80697982312774));
#21661=CARTESIAN_POINT('Ctrl Pts',(-10.3900811268588,32.7830083481296,3.90727035830497));
#21662=CARTESIAN_POINT('Ctrl Pts',(-10.3064370015652,32.8488643339236,4.12359767513566));
#21663=CARTESIAN_POINT('Ctrl Pts',(-10.2594208731612,32.9013952313582,4.23872376230597));
#21664=CARTESIAN_POINT('Ctrl Pts',(-10.175850299107,33.0452362980267,4.43536352549505));
#21665=CARTESIAN_POINT('Ctrl Pts',(-10.1409638178524,33.1289571391804,4.5139766435786));
#21666=CARTESIAN_POINT('Ctrl Pts',(-10.0784742720544,33.3396669565366,4.651959776916));
#21667=CARTESIAN_POINT('Ctrl Pts',(-10.0539479272323,33.4647551607016,4.70423708829085));
#21668=CARTESIAN_POINT('Ctrl Pts',(-10.0083714171123,33.7994478579441,4.80070434038827));
#21669=CARTESIAN_POINT('Ctrl Pts',(-9.99594466036069,34.0281657983108,4.82608437006716));
#21670=CARTESIAN_POINT('Ctrl Pts',(-9.99594466036069,34.2419663837872,4.82608437006716));
#21671=CARTESIAN_POINT('',(-10.923590324108,71.2419663837872,1.97108458241986));
#21672=CARTESIAN_POINT('',(-10.923590324108,52.7419663837872,1.97108458241986));
#21673=CARTESIAN_POINT('',(-9.9959446603607,71.2419663837872,4.82608437006716));
#21674=CARTESIAN_POINT('Ctrl Pts',(-9.9959446603607,71.2419663837872,4.82608437006716));
#21675=CARTESIAN_POINT('Ctrl Pts',(-9.9959446603607,71.4504917689704,4.82608437006716));
#21676=CARTESIAN_POINT('Ctrl Pts',(-10.0077566868326,71.6728033656151,4.80193693525385));
#21677=CARTESIAN_POINT('Ctrl Pts',(-10.0514082864556,72.0047784777117,4.7096530861913));
#21678=CARTESIAN_POINT('Ctrl Pts',(-10.0756462185106,72.1320608146004,4.65807430502912));
#21679=CARTESIAN_POINT('Ctrl Pts',(-10.1374662039434,72.3453273670303,4.52180422533563));
#21680=CARTESIAN_POINT('Ctrl Pts',(-10.1718457246957,72.4299633960725,4.44451147442909));
#21681=CARTESIAN_POINT('Ctrl Pts',(-10.2555080221753,72.5776598312471,4.24820764469124));
#21682=CARTESIAN_POINT('Ctrl Pts',(-10.3032505538534,72.632009574666,4.13161928458065));
#21683=CARTESIAN_POINT('Ctrl Pts',(-10.3875285520126,72.6993182274865,3.91403300809335));
#21684=CARTESIAN_POINT('Ctrl Pts',(-10.4245444036369,72.719076949585,3.8144402051162));
#21685=CARTESIAN_POINT('Ctrl Pts',(-10.4781093887339,72.7379457354566,3.66363531938785));
#21686=CARTESIAN_POINT('Ctrl Pts',(-10.4962229335872,72.7425013416222,3.6114176478374));
#21687=CARTESIAN_POINT('Ctrl Pts',(-10.5280640121862,72.7475581223538,3.51736037834474));
#21688=CARTESIAN_POINT('Ctrl Pts',(-10.5420579527565,72.7486976181121,3.47519424032086));
#21689=CARTESIAN_POINT('Ctrl Pts',(-10.5694311878668,72.7488007243628,3.39102934349868));
#21690=CARTESIAN_POINT('Ctrl Pts',(-10.5829014522237,72.7477675826252,3.34875319629768));
#21691=CARTESIAN_POINT('Ctrl Pts',(-10.6121572796231,72.7430091857572,3.25500200144533));
#21692=CARTESIAN_POINT('Ctrl Pts',(-10.6279303317184,72.7387110754265,3.20312145404714));
#21693=CARTESIAN_POINT('Ctrl Pts',(-10.6731143910354,72.7206077607173,3.05053014374159));
#21694=CARTESIAN_POINT('Ctrl Pts',(-10.701842760633,72.7013249659843,2.9480523535184));
#21695=CARTESIAN_POINT('Ctrl Pts',(-10.7610518579369,72.6362267971514,2.72511617846599));
#21696=CARTESIAN_POINT('Ctrl Pts',(-10.7905785607449,72.5843799091737,2.6049616514383));
#21697=CARTESIAN_POINT('Ctrl Pts',(-10.8386546030836,72.4419884523103,2.39667353469383));
#21698=CARTESIAN_POINT('Ctrl Pts',(-10.8567809666063,72.358608719572,2.31203741907976));
#21699=CARTESIAN_POINT('Ctrl Pts',(-10.8875104141335,72.1488438578622,2.1629881181418));
#21700=CARTESIAN_POINT('Ctrl Pts',(-10.8984634966878,72.024569430347,2.10600036378334));
#21701=CARTESIAN_POINT('Ctrl Pts',(-10.9189847308192,71.6831286857275,1.9976163626495));
#21702=CARTESIAN_POINT('Ctrl Pts',(-10.923590324108,71.4507884295547,1.97108458241986));
#21703=CARTESIAN_POINT('Ctrl Pts',(-10.923590324108,71.2419663837872,1.97108458241986));
#21704=CARTESIAN_POINT('',(-9.99594466036069,52.7419663837872,4.82608437006716));
#21705=CARTESIAN_POINT('',(-5.25018788601841,34.2419663837872,-9.77985312576347));
#21706=CARTESIAN_POINT('',(-7.6787957632255,34.2419663837872,-8.01536621912375));
#21707=CARTESIAN_POINT('Ctrl Pts',(-5.25018788601841,34.2419663837872,-9.77985312576347));
#21708=CARTESIAN_POINT('Ctrl Pts',(-5.25018788601841,34.0448673617023,-9.77985312576347));
#21709=CARTESIAN_POINT('Ctrl Pts',(-5.27139766293447,33.8362237308821,-9.76858698544027));
#21710=CARTESIAN_POINT('Ctrl Pts',(-5.35271121588592,33.5102351295624,-9.72419505176736));
#21711=CARTESIAN_POINT('Ctrl Pts',(-5.40127743435383,33.3781157666064,-9.69754414106396));
#21712=CARTESIAN_POINT('Ctrl Pts',(-5.52827355320222,33.1591718022933,-9.62562943077829));
#21713=CARTESIAN_POINT('Ctrl Pts',(-5.59916184636777,33.0725369802653,-9.58483321392156));
#21714=CARTESIAN_POINT('Ctrl Pts',(-5.78195336666643,32.9165975969892,-9.47587207959609));
#21715=CARTESIAN_POINT('Ctrl Pts',(-5.89204363899044,32.8583610724958,-9.4080946508133));
#21716=CARTESIAN_POINT('Ctrl Pts',(-6.09569829406892,32.7862330357376,-9.27705724932772));
#21717=CARTESIAN_POINT('Ctrl Pts',(-6.18840431445502,32.7652602373854,-9.21551810502964));
#21718=CARTESIAN_POINT('Ctrl Pts',(-6.32427199570981,32.7459057253595,-9.1223117695258));
#21719=CARTESIAN_POINT('Ctrl Pts',(-6.3695250930919,32.741377542263,-9.09077396133048));
#21720=CARTESIAN_POINT('Ctrl Pts',(-6.45047128243422,32.7363522396233,-9.03345866831879));
#21721=CARTESIAN_POINT('Ctrl Pts',(-6.48656990214715,32.7352238081385,-9.00757298827094));
#21722=CARTESIAN_POINT('Ctrl Pts',(-6.55818166766781,32.7351419995549,-8.95556862185794));
#21723=CARTESIAN_POINT('Ctrl Pts',(-6.59393135063778,32.7361860749744,-8.92927885654133));
#21724=CARTESIAN_POINT('Ctrl Pts',(-6.67278916372665,32.7409747471532,-8.87055895491593));
#21725=CARTESIAN_POINT('Ctrl Pts',(-6.7161255118715,32.7452987075796,-8.8377915352182));
#21726=CARTESIAN_POINT('Ctrl Pts',(-6.84285898440345,32.7635405469734,-8.7405089469008));
#21727=CARTESIAN_POINT('Ctrl Pts',(-6.9267465763262,32.7830083481296,-8.67414141820095));
#21728=CARTESIAN_POINT('Ctrl Pts',(-7.1066386244556,32.8488643339238,-8.52774231054221));
#21729=CARTESIAN_POINT('Ctrl Pts',(-7.20160125716801,32.9013952313585,-8.44745139782109));
#21730=CARTESIAN_POINT('Ctrl Pts',(-7.36279205769945,33.0452362980275,-8.30720603020093));
#21731=CARTESIAN_POINT('Ctrl Pts',(-7.42677706033752,33.1289571391814,-8.24973422540447));
#21732=CARTESIAN_POINT('Ctrl Pts',(-7.53869648681466,33.3396669565382,-8.14766400253443));
#21733=CARTESIAN_POINT('Ctrl Pts',(-7.58083610709224,33.4647551607036,-8.10818348483539));
#21734=CARTESIAN_POINT('Ctrl Pts',(-7.65849799963691,33.7994478579459,-8.03502762759727));
#21735=CARTESIAN_POINT('Ctrl Pts',(-7.6787957632255,34.0281657983116,-8.01536621912375));
#21736=CARTESIAN_POINT('Ctrl Pts',(-7.6787957632255,34.2419663837872,-8.01536621912375));
#21737=CARTESIAN_POINT('',(-5.25018788601841,71.2419663837872,-9.77985312576347));
#21738=CARTESIAN_POINT('',(-5.25018788601841,52.7419663837872,-9.77985312576347));
#21739=CARTESIAN_POINT('',(-7.6787957632255,71.2419663837872,-8.01536621912375));
#21740=CARTESIAN_POINT('Ctrl Pts',(-7.6787957632255,71.2419663837872,-8.01536621912375));
#21741=CARTESIAN_POINT('Ctrl Pts',(-7.6787957632255,71.4504917689704,-8.01536621912375));
#21742=CARTESIAN_POINT('Ctrl Pts',(-7.65948030491215,71.672803365615,-8.03406209159852));
#21743=CARTESIAN_POINT('Ctrl Pts',(-7.58520223502721,72.0047784777118,-8.10409450753371));
#21744=CARTESIAN_POINT('Ctrl Pts',(-7.5436378320136,72.1320608146008,-8.14308487068458));
#21745=CARTESIAN_POINT('Ctrl Pts',(-7.43314071083521,72.3453273670311,-8.24398894111832));
#21746=CARTESIAN_POINT('Ctrl Pts',(-7.37025479259382,72.4299633960733,-8.30057058192927));
#21747=CARTESIAN_POINT('Ctrl Pts',(-7.20941182785736,72.5776598312477,-8.44079937456552));
#21748=CARTESIAN_POINT('Ctrl Pts',(-7.11328296189318,72.6320095746664,-8.5222330050427));
#21749=CARTESIAN_POINT('Ctrl Pts',(-6.93238944946695,72.6993182274868,-8.6696240015494));
#21750=CARTESIAN_POINT('Ctrl Pts',(-6.84910959243269,72.7190769495851,-8.73560403708014));
#21751=CARTESIAN_POINT('Ctrl Pts',(-6.72223811387062,72.7379457354566,-8.8331486377262));
#21752=CARTESIAN_POINT('Ctrl Pts',(-6.67817355026513,72.7425013416222,-8.86651179050778));
#21753=CARTESIAN_POINT('Ctrl Pts',(-6.59855920561544,72.7475581223538,-8.92585975051296));
#21754=CARTESIAN_POINT('Ctrl Pts',(-6.56278119073531,72.7486976181121,-8.95219883211757));
#21755=CARTESIAN_POINT('Ctrl Pts',(-6.49119441201008,72.7488007243628,-9.00424070918861));
#21756=CARTESIAN_POINT('Ctrl Pts',(-6.45514994733573,72.7477675826252,-9.03011573982327));
#21757=CARTESIAN_POINT('Ctrl Pts',(-6.3750278104121,72.7430091857572,-9.08691039756328));
#21758=CARTESIAN_POINT('Ctrl Pts',(-6.33056061889071,72.7387110754265,-9.11794343236385));
#21759=CARTESIAN_POINT('Ctrl Pts',(-6.19940030109833,72.7206077607173,-9.20806933448834));
#21760=CARTESIAN_POINT('Ctrl Pts',(-6.11081568535744,72.7013249659842,-9.26705901632166));
#21761=CARTESIAN_POINT('Ctrl Pts',(-5.9170874006442,72.6362267971512,-9.39226128088876));
#21762=CARTESIAN_POINT('Ctrl Pts',(-5.81193790770756,72.5843799091733,-9.45747263480172));
#21763=CARTESIAN_POINT('Ctrl Pts',(-5.62870045111564,72.4419884523096,-9.56756023594614));
#21764=CARTESIAN_POINT('Ctrl Pts',(-5.55380807622163,72.358608719571,-9.61095343015381));
#21765=CARTESIAN_POINT('Ctrl Pts',(-5.42154968882878,72.1488438578607,-9.68623763845631));
#21766=CARTESIAN_POINT('Ctrl Pts',(-5.37073580234716,72.0245694303451,-9.71426482356116));
#21767=CARTESIAN_POINT('Ctrl Pts',(-5.27399790189915,71.6831286857257,-9.76727417527282));
#21768=CARTESIAN_POINT('Ctrl Pts',(-5.25018788601841,71.4507884295538,-9.77985312576347));
#21769=CARTESIAN_POINT('Ctrl Pts',(-5.25018788601841,71.2419663837872,-9.77985312576347));
#21770=CARTESIAN_POINT('',(-7.6787957632255,52.7419663837872,-8.01536621912375));
#21771=CARTESIAN_POINT('Origin',(0.,275.,0.));
#21772=CARTESIAN_POINT('',(-1.35935794705356E-15,76.9512489600658,11.1));
#21773=CARTESIAN_POINT('Origin',(0.,76.9512489600658,0.));
#21774=CARTESIAN_POINT('',(-1.20009601631982E-15,261.7,11.1));
#21775=CARTESIAN_POINT('',(-1.35935794705356E-15,275.,11.1));
#21776=CARTESIAN_POINT('',(-3.1,264.8,10.6583300755794));
#21777=CARTESIAN_POINT('Ctrl Pts',(-2.22044604925031E-15,261.7,11.1));
#21778=CARTESIAN_POINT('Ctrl Pts',(-0.391454890651857,261.7,11.1));
#21779=CARTESIAN_POINT('Ctrl Pts',(-0.807604729509082,261.77865672835,11.0772325011544));
#21780=CARTESIAN_POINT('Ctrl Pts',(-1.57079416556834,262.095680105178,10.9949948149978));
#21781=CARTESIAN_POINT('Ctrl Pts',(-1.91799680212002,262.333934758763,10.9366096412455));
#21782=CARTESIAN_POINT('Ctrl Pts',(-2.46612584114063,262.882063797784,10.8261904693255));
#21783=CARTESIAN_POINT('Ctrl Pts',(-2.70433342241585,263.229241539378,10.7667771783582));
#21784=CARTESIAN_POINT('Ctrl Pts',(-3.02132222583929,263.992341466568,10.682159098241));
#21785=CARTESIAN_POINT('Ctrl Pts',(-3.09999999999999,264.408458543047,10.6583300755794));
#21786=CARTESIAN_POINT('Ctrl Pts',(-3.1,264.8,10.6583300755794));
#21787=CARTESIAN_POINT('',(-1.2694849553589E-15,267.9,11.1));
#21788=CARTESIAN_POINT('Ctrl Pts',(-3.09999999999999,264.8,10.6583300755794));
#21789=CARTESIAN_POINT('Ctrl Pts',(-3.09999999999999,265.191541456953,10.6583300755794));
#21790=CARTESIAN_POINT('Ctrl Pts',(-3.02132222583929,265.607658533432,10.682159098241));
#21791=CARTESIAN_POINT('Ctrl Pts',(-2.70433342241585,266.370758460622,10.7667771783582));
#21792=CARTESIAN_POINT('Ctrl Pts',(-2.46612584114063,266.717936202216,10.8261904693255));
#21793=CARTESIAN_POINT('Ctrl Pts',(-1.91799680212002,267.266065241237,10.9366096412455));
#21794=CARTESIAN_POINT('Ctrl Pts',(-1.57079416556834,267.504319894822,10.9949948149978));
#21795=CARTESIAN_POINT('Ctrl Pts',(-0.807604729509082,267.821343271651,
11.0772325011544));
#21796=CARTESIAN_POINT('Ctrl Pts',(-0.391454890651854,267.9,11.1));
#21797=CARTESIAN_POINT('Ctrl Pts',(0.,267.9,11.1));
#21798=CARTESIAN_POINT('',(0.,274.5,11.1));
#21799=CARTESIAN_POINT('',(-1.35935794705356E-15,275.,11.1));
#21800=CARTESIAN_POINT('Origin',(0.,274.5,0.));
#21801=CARTESIAN_POINT('',(3.09999999999999,264.8,10.6583300755794));
#21802=CARTESIAN_POINT('Ctrl Pts',(1.04083408558608E-15,267.9,11.1));
#21803=CARTESIAN_POINT('Ctrl Pts',(0.391454890651855,267.9,11.1));
#21804=CARTESIAN_POINT('Ctrl Pts',(0.807604729509082,267.821343271651,11.0772325011544));
#21805=CARTESIAN_POINT('Ctrl Pts',(1.57079416556834,267.504319894822,10.9949948149978));
#21806=CARTESIAN_POINT('Ctrl Pts',(1.91799680212002,267.266065241237,10.9366096412455));
#21807=CARTESIAN_POINT('Ctrl Pts',(2.46612584114063,266.717936202216,10.8261904693255));
#21808=CARTESIAN_POINT('Ctrl Pts',(2.70433342241585,266.370758460622,10.7667771783582));
#21809=CARTESIAN_POINT('Ctrl Pts',(3.02132222583929,265.607658533432,10.682159098241));
#21810=CARTESIAN_POINT('Ctrl Pts',(3.1,265.191541456953,10.6583300755794));
#21811=CARTESIAN_POINT('Ctrl Pts',(3.1,264.8,10.6583300755794));
#21812=CARTESIAN_POINT('Ctrl Pts',(3.09999999999999,264.8,10.6583300755794));
#21813=CARTESIAN_POINT('Ctrl Pts',(3.09999999999999,264.408458543047,10.6583300755794));
#21814=CARTESIAN_POINT('Ctrl Pts',(3.02132222583929,263.992341466568,10.682159098241));
#21815=CARTESIAN_POINT('Ctrl Pts',(2.70433342241585,263.229241539378,10.7667771783582));
#21816=CARTESIAN_POINT('Ctrl Pts',(2.46612584114063,262.882063797784,10.8261904693255));
#21817=CARTESIAN_POINT('Ctrl Pts',(1.91799680212002,262.333934758763,10.9366096412455));
#21818=CARTESIAN_POINT('Ctrl Pts',(1.57079416556834,262.095680105178,10.9949948149978));
#21819=CARTESIAN_POINT('Ctrl Pts',(0.807604729509083,261.77865672835,11.0772325011544));
#21820=CARTESIAN_POINT('Ctrl Pts',(0.391454890651857,261.7,11.1));
#21821=CARTESIAN_POINT('Ctrl Pts',(2.91433543964104E-15,261.7,11.1));
#21822=CARTESIAN_POINT('',(0.,267.9,-11.1));
#21823=CARTESIAN_POINT('',(-3.09999999999999,264.8,-10.6583300755794));
#21824=CARTESIAN_POINT('Ctrl Pts',(-4.85722573273506E-16,267.9,-11.1));
#21825=CARTESIAN_POINT('Ctrl Pts',(-0.391454890651855,267.9,-11.1));
#21826=CARTESIAN_POINT('Ctrl Pts',(-0.807604729509082,267.821343271651,
-11.0772325011544));
#21827=CARTESIAN_POINT('Ctrl Pts',(-1.57079416556834,267.504319894822,-10.9949948149978));
#21828=CARTESIAN_POINT('Ctrl Pts',(-1.91799680212002,267.266065241237,-10.9366096412455));
#21829=CARTESIAN_POINT('Ctrl Pts',(-2.46612584114063,266.717936202216,-10.8261904693255));
#21830=CARTESIAN_POINT('Ctrl Pts',(-2.70433342241585,266.370758460622,-10.7667771783582));
#21831=CARTESIAN_POINT('Ctrl Pts',(-3.02132222583929,265.607658533432,-10.682159098241));
#21832=CARTESIAN_POINT('Ctrl Pts',(-3.09999999999999,265.191541456953,-10.6583300755794));
#21833=CARTESIAN_POINT('Ctrl Pts',(-3.09999999999999,264.8,-10.6583300755794));
#21834=CARTESIAN_POINT('Ctrl Pts',(-3.09999999999999,264.8,-10.6583300755794));
#21835=CARTESIAN_POINT('Ctrl Pts',(-3.09999999999999,264.408458543047,-10.6583300755794));
#21836=CARTESIAN_POINT('Ctrl Pts',(-3.02132222583929,263.992341466568,-10.682159098241));
#21837=CARTESIAN_POINT('Ctrl Pts',(-2.70433342241585,263.229241539378,-10.7667771783582));
#21838=CARTESIAN_POINT('Ctrl Pts',(-2.46612584114063,262.882063797784,-10.8261904693255));
#21839=CARTESIAN_POINT('Ctrl Pts',(-1.91799680212002,262.333934758763,-10.9366096412455));
#21840=CARTESIAN_POINT('Ctrl Pts',(-1.57079416556834,262.095680105178,-10.9949948149978));
#21841=CARTESIAN_POINT('Ctrl Pts',(-0.807604729509082,261.77865672835,-11.0772325011544));
#21842=CARTESIAN_POINT('Ctrl Pts',(-0.391454890651854,261.7,-11.1));
#21843=CARTESIAN_POINT('Ctrl Pts',(0.391454890651854,261.7,-11.1));
#21844=CARTESIAN_POINT('Ctrl Pts',(0.807604729509082,261.77865672835,-11.0772325011544));
#21845=CARTESIAN_POINT('Ctrl Pts',(1.57079416556834,262.095680105178,-10.9949948149978));
#21846=CARTESIAN_POINT('Ctrl Pts',(1.91799680212002,262.333934758763,-10.9366096412455));
#21847=CARTESIAN_POINT('Ctrl Pts',(2.46612584114063,262.882063797784,-10.8261904693255));
#21848=CARTESIAN_POINT('Ctrl Pts',(2.70433342241585,263.229241539378,-10.7667771783582));
#21849=CARTESIAN_POINT('Ctrl Pts',(3.02132222583929,263.992341466568,-10.682159098241));
#21850=CARTESIAN_POINT('Ctrl Pts',(3.09999999999999,264.408458543047,-10.6583300755794));
#21851=CARTESIAN_POINT('Ctrl Pts',(3.09999999999999,265.191541456953,-10.6583300755794));
#21852=CARTESIAN_POINT('Ctrl Pts',(3.02132222583929,265.607658533432,-10.682159098241));
#21853=CARTESIAN_POINT('Ctrl Pts',(2.70433342241585,266.370758460622,-10.7667771783582));
#21854=CARTESIAN_POINT('Ctrl Pts',(2.46612584114063,266.717936202216,-10.8261904693255));
#21855=CARTESIAN_POINT('Ctrl Pts',(1.91799680212002,267.266065241237,-10.9366096412455));
#21856=CARTESIAN_POINT('Ctrl Pts',(1.57079416556834,267.504319894822,-10.9949948149978));
#21857=CARTESIAN_POINT('Ctrl Pts',(0.807604729509083,267.821343271651,-11.0772325011544));
#21858=CARTESIAN_POINT('Ctrl Pts',(0.391454890651858,267.9,-11.1));
#21859=CARTESIAN_POINT('Ctrl Pts',(3.67761376907083E-15,267.9,-11.1));
#21860=CARTESIAN_POINT('Origin',(0.,275.,0.));
#21861=CARTESIAN_POINT('',(0.,0.499999999999945,11.1));
#21862=CARTESIAN_POINT('',(-1.35935794705356E-15,0.499999999999945,-11.1));
#21863=CARTESIAN_POINT('Origin',(0.,0.499999999999945,0.));
#21864=CARTESIAN_POINT('Origin',(0.,0.499999999999945,0.));
#21865=CARTESIAN_POINT('',(1.61143898433164E-13,2.67704306348694,11.1));
#21866=CARTESIAN_POINT('',(-1.35935794705356E-15,275.,11.1));
#21867=CARTESIAN_POINT('',(-2.0260462879878E-12,7.32295697727983,11.1));
#21868=CARTESIAN_POINT('Ctrl Pts',(3.23647154813382E-13,2.67704306348694,
11.1));
#21869=CARTESIAN_POINT('Ctrl Pts',(-0.273139581690495,2.67704308193317,
11.1));
#21870=CARTESIAN_POINT('Ctrl Pts',(-0.544517384377054,2.72153833743136,
11.0896641648894));
#21871=CARTESIAN_POINT('Ctrl Pts',(-1.10258484109494,2.91067862507553,11.0491875912365));
#21872=CARTESIAN_POINT('Ctrl Pts',(-1.3798661147451,3.06856373870345,11.0165275551973));
#21873=CARTESIAN_POINT('Ctrl Pts',(-1.84282580329821,3.47012918997237,10.948317869715));
#21874=CARTESIAN_POINT('Ctrl Pts',(-2.02918140675796,3.7055024182498,10.9138310665725));
#21875=CARTESIAN_POINT('Ctrl Pts',(-2.29556418563575,4.22355226854262,10.8608471933831));
#21876=CARTESIAN_POINT('Ctrl Pts',(-2.3775175883224,4.49913306003288,10.8424265102952));
#21877=CARTESIAN_POINT('Ctrl Pts',(-2.40517323731289,4.78410483624288,10.8362881882372));
#21878=CARTESIAN_POINT('Ctrl Pts',(-2.42308944027353,4.96871855412709,10.8323115893201));
#21879=CARTESIAN_POINT('Ctrl Pts',(-2.41796202305408,5.15442416696364,10.8334796125597));
#21880=CARTESIAN_POINT('Ctrl Pts',(-2.36183470646002,5.5218723530959,10.8458548618846));
#21881=CARTESIAN_POINT('Ctrl Pts',(-2.3109127065596,5.70137997051123,10.8570313240313));
#21882=CARTESIAN_POINT('Ctrl Pts',(-2.11813065645628,6.15860457306728,10.8967269208308));
#21883=CARTESIAN_POINT('Ctrl Pts',(-1.94101086541288,6.41571203975272,10.9312778707514));
#21884=CARTESIAN_POINT('Ctrl Pts',(-1.49402342882342,6.85125097027356,11.0013588285694));
#21885=CARTESIAN_POINT('Ctrl Pts',(-1.22720905280096,7.02401263594798,11.0358642385009));
#21886=CARTESIAN_POINT('Ctrl Pts',(-0.642145747279439,7.26002789053428,
11.0852910865185));
#21887=CARTESIAN_POINT('Ctrl Pts',(-0.330182188115768,7.32101004289588,
11.0995604536001));
#21888=CARTESIAN_POINT('Ctrl Pts',(-0.0100813466862662,7.32294187220753,
11.0999965668345));
#21889=CARTESIAN_POINT('Ctrl Pts',(-0.00504035649498059,7.32295707066767,
11.1));
#21890=CARTESIAN_POINT('Ctrl Pts',(-4.05073321802854E-12,7.32295697727983,
11.1));
#21891=CARTESIAN_POINT('',(0.,12.4487510399342,11.1));
#21892=CARTESIAN_POINT('',(-1.35935794705356E-15,275.,11.1));
#21893=CARTESIAN_POINT('Origin',(0.,12.4487510399342,0.));
#21894=CARTESIAN_POINT('',(2.41562897926683,5.,10.833962185393));
#21895=CARTESIAN_POINT('Ctrl Pts',(-4.05073321802854E-12,7.32295697727983,
11.1));
#21896=CARTESIAN_POINT('Ctrl Pts',(0.315495834708401,7.32295113176525,11.1000000000001));
#21897=CARTESIAN_POINT('Ctrl Pts',(0.628508866369116,7.26353532669138,11.0860850371572));
#21898=CARTESIAN_POINT('Ctrl Pts',(1.21451436236122,7.03104316540582,11.0372796619423));
#21899=CARTESIAN_POINT('Ctrl Pts',(1.48278165110063,6.85960869665576,11.0029086057863));
#21900=CARTESIAN_POINT('Ctrl Pts',(1.92338507228345,6.43522915122724,10.9342333167844));
#21901=CARTESIAN_POINT('Ctrl Pts',(2.09658178139581,6.19108347331183,10.9009068044498));
#21902=CARTESIAN_POINT('Ctrl Pts',(2.3348660806695,5.65953558717099,10.852306679531));
#21903=CARTESIAN_POINT('Ctrl Pts',(2.40154335470469,5.38013985460967,10.8371002996985));
#21904=CARTESIAN_POINT('Ctrl Pts',(2.41496509132228,5.06293051253712,10.8341102760105));
#21905=CARTESIAN_POINT('Ctrl Pts',(2.41562898203172,5.03144629441105,10.8339621847766));
#21906=CARTESIAN_POINT('Ctrl Pts',(2.41562897926683,5.,10.833962185393));
#21907=CARTESIAN_POINT('Ctrl Pts',(2.41562897926683,5.,10.833962185393));
#21908=CARTESIAN_POINT('Ctrl Pts',(2.41562895648218,4.74086038603115,10.8339621904733));
#21909=CARTESIAN_POINT('Ctrl Pts',(2.37058559554881,4.48429608284729,10.8442778599772));
#21910=CARTESIAN_POINT('Ctrl Pts',(2.17946594106486,3.95311954848045,10.8844424518853));
#21911=CARTESIAN_POINT('Ctrl Pts',(2.01939079066006,3.69060671315312,10.9167481416166));
#21912=CARTESIAN_POINT('Ctrl Pts',(1.60207378032625,3.23423850139877,10.9858781650619));
#21913=CARTESIAN_POINT('Ctrl Pts',(1.3455459736091,3.0467729086828,11.0218702685321));
#21914=CARTESIAN_POINT('Ctrl Pts',(0.772856356127114,2.7777494777404,11.0768259913659));
#21915=CARTESIAN_POINT('Ctrl Pts',(0.461192262550163,2.69922142801988,11.094988270665));
#21916=CARTESIAN_POINT('Ctrl Pts',(0.0951098358302787,2.67839196589101,
11.0996944994446));
#21917=CARTESIAN_POINT('Ctrl Pts',(0.0475282448567165,2.67704306027716,
11.1));
#21918=CARTESIAN_POINT('Ctrl Pts',(3.23647154813382E-13,2.67704306348694,
11.1));
#21919=CARTESIAN_POINT('',(-2.71871589410712E-15,7.32295693650353,-11.1));
#21920=CARTESIAN_POINT('Ctrl Pts',(-2.46904150249686E-15,7.32295693650353,
-11.1));
#21921=CARTESIAN_POINT('Ctrl Pts',(-0.0695652818990985,7.32295783550982,
-11.1));
#21922=CARTESIAN_POINT('Ctrl Pts',(-0.139218809299037,7.32006775869429,
-11.0993450131274));
#21923=CARTESIAN_POINT('Ctrl Pts',(-0.528466789920203,7.28759395137216,
-11.0920220652185));
#21924=CARTESIAN_POINT('Ctrl Pts',(-0.839196549011331,7.20011126493925,
-11.0719290301748));
#21925=CARTESIAN_POINT('Ctrl Pts',(-1.40169375654943,6.91581877804573,-11.0146835965512));
#21926=CARTESIAN_POINT('Ctrl Pts',(-1.65013536422944,6.7237844228964,-10.9786031937536));
#21927=CARTESIAN_POINT('Ctrl Pts',(-2.04573187848749,6.26842859693051,-10.9115934145661));
#21928=CARTESIAN_POINT('Ctrl Pts',(-2.19481020238894,6.01339934425637,-10.8812914141919));
#21929=CARTESIAN_POINT('Ctrl Pts',(-2.38466733146137,5.46687720810133,-10.8412405251123));
#21930=CARTESIAN_POINT('Ctrl Pts',(-2.42638928271567,5.18274028883403,-10.8315657047934));
#21931=CARTESIAN_POINT('Ctrl Pts',(-2.39970912117631,4.6023397708397,-10.8375084426288));
#21932=CARTESIAN_POINT('Ctrl Pts',(-2.32789728802446,4.31417905623201,-10.8538969744193));
#21933=CARTESIAN_POINT('Ctrl Pts',(-2.0724135232689,3.7677138426677,-10.9056366497519));
#21934=CARTESIAN_POINT('Ctrl Pts',(-1.88647098366285,3.51801820624971,-10.940955305182));
#21935=CARTESIAN_POINT('Ctrl Pts',(-1.42614298609066,3.10012773169153,-11.0105048755359));
#21936=CARTESIAN_POINT('Ctrl Pts',(-1.15427898086522,2.93682125994773,-11.0438097881092));
#21937=CARTESIAN_POINT('Ctrl Pts',(-0.557940747205909,2.71881889702648,
-11.0900629860885));
#21938=CARTESIAN_POINT('Ctrl Pts',(-0.238737740968463,2.66797692828207,
-11.1020514614943));
#21939=CARTESIAN_POINT('Ctrl Pts',(0.0814759967561537,2.67836337071254,
-11.0997009717358));
#21940=CARTESIAN_POINT('Ctrl Pts',(0.285421015271941,2.68497852473075,-11.0982039382833));
#21941=CARTESIAN_POINT('Ctrl Pts',(0.487856497256365,2.71645669516471,-11.0910086113376));
#21942=CARTESIAN_POINT('Ctrl Pts',(0.877921673005148,2.8271378442534,-11.0669392231544));
#21943=CARTESIAN_POINT('Ctrl Pts',(1.06491376579154,2.90576754946889,-11.0501997293928));
#21944=CARTESIAN_POINT('Ctrl Pts',(1.50637405997121,3.15962708068845,-11.0005827675453));
#21945=CARTESIAN_POINT('Ctrl Pts',(1.74119128221293,3.36171267697428,-10.9642651821397));
#21946=CARTESIAN_POINT('Ctrl Pts',(2.10874780489197,3.831472605075,-10.8993594960467));
#21947=CARTESIAN_POINT('Ctrl Pts',(2.24332570855584,4.09096781536863,-10.8712685160658));
#21948=CARTESIAN_POINT('Ctrl Pts',(2.40531152247706,4.64373711172344,-10.8365681858915));
#21949=CARTESIAN_POINT('Ctrl Pts',(2.43274503947083,4.9297892674136,-10.8301680767129));
#21950=CARTESIAN_POINT('Ctrl Pts',(2.37669341236812,5.51144009685063,-10.8426098557504));
#21951=CARTESIAN_POINT('Ctrl Pts',(2.28908482971336,5.79836274682849,-10.8623397100488));
#21952=CARTESIAN_POINT('Ctrl Pts',(2.00213836415185,6.33610283283957,-10.9189700913053));
#21953=CARTESIAN_POINT('Ctrl Pts',(1.8006305505284,6.57828056462836,-10.9557149186307));
#21954=CARTESIAN_POINT('Ctrl Pts',(1.31295487334744,6.97413780170986,-11.0248581802782));
#21955=CARTESIAN_POINT('Ctrl Pts',(1.03053677251028,7.123233785964,-11.0562637699774));
#21956=CARTESIAN_POINT('Ctrl Pts',(0.490350610681507,7.28700460364381,-11.0916840411728));
#21957=CARTESIAN_POINT('Ctrl Pts',(0.245725806500237,7.32295376093894,-11.1));
#21958=CARTESIAN_POINT('Ctrl Pts',(-2.46904150249686E-15,7.32295693650353,
-11.1));
#21959=CARTESIAN_POINT('Origin',(0.,275.,0.));
#21960=CARTESIAN_POINT('',(0.,275.,10.6));
#21961=CARTESIAN_POINT('Origin',(0.,275.,0.));
#21962=CARTESIAN_POINT('',(-1.18790592559677E-15,275.,-9.69998799999994));
#21963=CARTESIAN_POINT('Origin',(0.,275.,0.));
#21964=CARTESIAN_POINT('Origin',(0.,0.,0.));
#21965=CARTESIAN_POINT('',(-1.2981256070962E-15,-4.85722573273506E-16,-10.6));
#21966=CARTESIAN_POINT('Origin',(0.,0.,0.));
#21967=CARTESIAN_POINT('',(0.,0.,9.70000000000007));
#21968=CARTESIAN_POINT('Origin',(0.,0.,0.));
#21969=CARTESIAN_POINT('Origin',(0.,0.,0.));
#21970=CARTESIAN_POINT('',(0.,0.500000000000066,9.2));
#21971=CARTESIAN_POINT('',(-1.12667505521557E-15,0.500000000000066,-9.2));
#21972=CARTESIAN_POINT('Origin',(0.,0.500000000000066,0.));
#21973=CARTESIAN_POINT('',(-5.63337527607783E-16,3.,-9.2));
#21974=CARTESIAN_POINT('',(-1.12667505521557E-15,0.,-9.2));
#21975=CARTESIAN_POINT('',(-2.,5.,-8.97997772825746));
#21976=CARTESIAN_POINT('Ctrl Pts',(1.38777878078145E-16,3.,-9.2));
#21977=CARTESIAN_POINT('Ctrl Pts',(-0.251982495387346,3.,-9.2));
#21978=CARTESIAN_POINT('Ctrl Pts',(-0.520217657456257,3.05052306683097,
-9.18860399767844));
#21979=CARTESIAN_POINT('Ctrl Pts',(-1.0127456170646,3.25488309906895,-9.1474267505225));
#21980=CARTESIAN_POINT('Ctrl Pts',(-1.23710338548845,3.40867626074226,-9.11820719093608));
#21981=CARTESIAN_POINT('Ctrl Pts',(-1.59133769071452,3.76291056596832,-9.06309972244743));
#21982=CARTESIAN_POINT('Ctrl Pts',(-1.7451199392152,3.98726244660274,-9.0335726503792));
#21983=CARTESIAN_POINT('Ctrl Pts',(-1.94947204040866,4.479769809412,-8.99168712872246));
#21984=CARTESIAN_POINT('Ctrl Pts',(-2.,4.74799765525699,-8.97997772825746));
#21985=CARTESIAN_POINT('Ctrl Pts',(-2.,5.,-8.97997772825746));
#21986=CARTESIAN_POINT('',(-6.67420936166391E-16,7.,-9.2));
#21987=CARTESIAN_POINT('Ctrl Pts',(-2.,5.,-8.97997772825746));
#21988=CARTESIAN_POINT('Ctrl Pts',(-2.,5.25200234474301,-8.97997772825746));
#21989=CARTESIAN_POINT('Ctrl Pts',(-1.94947204040866,5.520230190588,-8.99168712872246));
#21990=CARTESIAN_POINT('Ctrl Pts',(-1.7451199392152,6.01273755339726,-9.0335726503792));
#21991=CARTESIAN_POINT('Ctrl Pts',(-1.59133769071452,6.23708943403168,-9.06309972244743));
#21992=CARTESIAN_POINT('Ctrl Pts',(-1.23710338548845,6.59132373925774,-9.11820719093608));
#21993=CARTESIAN_POINT('Ctrl Pts',(-1.0127456170646,6.74511690093105,-9.1474267505225));
#21994=CARTESIAN_POINT('Ctrl Pts',(-0.520217657456257,6.94947693316903,
-9.18860399767844));
#21995=CARTESIAN_POINT('Ctrl Pts',(-0.251982495387347,7.,-9.2));
#21996=CARTESIAN_POINT('Ctrl Pts',(-6.93889390390723E-16,7.,-9.2));
#21997=CARTESIAN_POINT('',(-1.01436563136175E-15,261.7,-9.2));
#21998=CARTESIAN_POINT('',(-1.12667505521557E-15,0.,-9.2));
#21999=CARTESIAN_POINT('',(-3.09999999999999,264.8,-8.66198591548151));
#22000=CARTESIAN_POINT('Ctrl Pts',(0.,261.7,-9.2));
#22001=CARTESIAN_POINT('Ctrl Pts',(-0.392492181867812,261.7,-9.2));
#22002=CARTESIAN_POINT('Ctrl Pts',(-0.809098032285487,261.779064419326,
-9.17242354783845));
#22003=CARTESIAN_POINT('Ctrl Pts',(-1.57202652449705,262.096405395141,-9.07285654990429));
#22004=CARTESIAN_POINT('Ctrl Pts',(-1.91858114764766,262.334519104291,-9.00212872931236));
#22005=CARTESIAN_POINT('Ctrl Pts',(-2.46561371815086,262.881551674794,-8.86792542274352));
#22006=CARTESIAN_POINT('Ctrl Pts',(-2.70362524494473,263.228053521236,-8.79535506867642));
#22007=CARTESIAN_POINT('Ctrl Pts',(-3.02088992440016,263.990785821449,-8.69149502149012));
#22008=CARTESIAN_POINT('Ctrl Pts',(-3.09999999999999,264.407317173429,-8.66198591548151));
#22009=CARTESIAN_POINT('Ctrl Pts',(-3.09999999999999,264.8,-8.66198591548151));
#22010=CARTESIAN_POINT('',(-2.12458865598691E-15,267.9,-9.2));
#22011=CARTESIAN_POINT('Ctrl Pts',(-3.1,264.8,-8.66198591548151));
#22012=CARTESIAN_POINT('Ctrl Pts',(-3.1,265.192682826571,-8.66198591548151));
#22013=CARTESIAN_POINT('Ctrl Pts',(-3.02088992440016,265.609214178551,-8.69149502149013));
#22014=CARTESIAN_POINT('Ctrl Pts',(-2.70362524494473,266.371946478764,-8.79535506867642));
#22015=CARTESIAN_POINT('Ctrl Pts',(-2.46561371815086,266.718448325206,-8.86792542274352));
#22016=CARTESIAN_POINT('Ctrl Pts',(-1.91858114764766,267.265480895709,-9.00212872931236));
#22017=CARTESIAN_POINT('Ctrl Pts',(-1.57202652449705,267.503594604859,-9.07285654990429));
#22018=CARTESIAN_POINT('Ctrl Pts',(-0.809098032285488,267.820935580675,
-9.17242354783845));
#22019=CARTESIAN_POINT('Ctrl Pts',(-0.392492181867816,267.9,-9.2));
#22020=CARTESIAN_POINT('Ctrl Pts',(-3.53883589099269E-15,267.9,-9.2));
#22021=CARTESIAN_POINT('',(-1.12667505521557E-15,274.500012,-9.2));
#22022=CARTESIAN_POINT('',(-1.12667505521557E-15,0.,-9.2));
#22023=CARTESIAN_POINT('Origin',(0.,274.500012,0.));
#22024=CARTESIAN_POINT('',(3.09999999999999,264.8,-8.66198591548151));
#22025=CARTESIAN_POINT('Ctrl Pts',(-3.2612801348364E-15,267.9,-9.2));
#22026=CARTESIAN_POINT('Ctrl Pts',(0.392492181867809,267.9,-9.2));
#22027=CARTESIAN_POINT('Ctrl Pts',(0.809098032285487,267.820935580675,-9.17242354783845));
#22028=CARTESIAN_POINT('Ctrl Pts',(1.57202652449705,267.503594604859,-9.07285654990429));
#22029=CARTESIAN_POINT('Ctrl Pts',(1.91858114764766,267.265480895709,-9.00212872931236));
#22030=CARTESIAN_POINT('Ctrl Pts',(2.46561371815086,266.718448325206,-8.86792542274352));
#22031=CARTESIAN_POINT('Ctrl Pts',(2.70362524494473,266.371946478764,-8.79535506867642));
#22032=CARTESIAN_POINT('Ctrl Pts',(3.02088992440016,265.609214178551,-8.69149502149013));
#22033=CARTESIAN_POINT('Ctrl Pts',(3.09999999999999,265.192682826571,-8.66198591548151));
#22034=CARTESIAN_POINT('Ctrl Pts',(3.09999999999999,264.8,-8.66198591548151));
#22035=CARTESIAN_POINT('Ctrl Pts',(3.09999999999999,264.8,-8.66198591548151));
#22036=CARTESIAN_POINT('Ctrl Pts',(3.09999999999999,264.407317173429,-8.66198591548151));
#22037=CARTESIAN_POINT('Ctrl Pts',(3.02088992440016,263.990785821449,-8.69149502149012));
#22038=CARTESIAN_POINT('Ctrl Pts',(2.70362524494473,263.228053521236,-8.79535506867642));
#22039=CARTESIAN_POINT('Ctrl Pts',(2.46561371815086,262.881551674794,-8.86792542274352));
#22040=CARTESIAN_POINT('Ctrl Pts',(1.91858114764766,262.334519104291,-9.00212872931236));
#22041=CARTESIAN_POINT('Ctrl Pts',(1.57202652449705,262.096405395141,-9.07285654990429));
#22042=CARTESIAN_POINT('Ctrl Pts',(0.809098032285487,261.779064419326,-9.17242354783845));
#22043=CARTESIAN_POINT('Ctrl Pts',(0.392492181867812,261.7,-9.2));
#22044=CARTESIAN_POINT('Ctrl Pts',(3.12250225675825E-16,261.7,-9.2));
#22045=CARTESIAN_POINT('',(2.,5.,-8.97997772825746));
#22046=CARTESIAN_POINT('Ctrl Pts',(-1.38777878078145E-16,7.,-9.2));
#22047=CARTESIAN_POINT('Ctrl Pts',(0.251982495387346,7.,-9.2));
#22048=CARTESIAN_POINT('Ctrl Pts',(0.520217657456257,6.94947693316903,-9.18860399767844));
#22049=CARTESIAN_POINT('Ctrl Pts',(1.0127456170646,6.74511690093105,-9.1474267505225));
#22050=CARTESIAN_POINT('Ctrl Pts',(1.23710338548845,6.59132373925774,-9.11820719093608));
#22051=CARTESIAN_POINT('Ctrl Pts',(1.59133769071451,6.23708943403168,-9.06309972244743));
#22052=CARTESIAN_POINT('Ctrl Pts',(1.7451199392152,6.01273755339726,-9.0335726503792));
#22053=CARTESIAN_POINT('Ctrl Pts',(1.94947204040866,5.520230190588,-8.99168712872246));
#22054=CARTESIAN_POINT('Ctrl Pts',(2.,5.252002344743,-8.97997772825746));
#22055=CARTESIAN_POINT('Ctrl Pts',(2.,5.,-8.97997772825746));
#22056=CARTESIAN_POINT('Ctrl Pts',(2.,5.,-8.97997772825746));
#22057=CARTESIAN_POINT('Ctrl Pts',(2.,4.74799765525699,-8.97997772825746));
#22058=CARTESIAN_POINT('Ctrl Pts',(1.94947204040866,4.479769809412,-8.99168712872246));
#22059=CARTESIAN_POINT('Ctrl Pts',(1.7451199392152,3.98726244660274,-9.0335726503792));
#22060=CARTESIAN_POINT('Ctrl Pts',(1.59133769071452,3.76291056596832,-9.06309972244743));
#22061=CARTESIAN_POINT('Ctrl Pts',(1.23710338548845,3.40867626074226,-9.11820719093608));
#22062=CARTESIAN_POINT('Ctrl Pts',(1.0127456170646,3.25488309906895,-9.1474267505225));
#22063=CARTESIAN_POINT('Ctrl Pts',(0.520217657456257,3.05052306683097,-9.18860399767844));
#22064=CARTESIAN_POINT('Ctrl Pts',(0.251982495387346,3.,-9.2));
#22065=CARTESIAN_POINT('Ctrl Pts',(6.93889390390723E-17,3.,-9.2));
#22066=CARTESIAN_POINT('Origin',(0.,0.500000000000066,0.));
#22067=CARTESIAN_POINT('',(0.,3.,9.2));
#22068=CARTESIAN_POINT('',(-2.,5.,8.97997772825746));
#22069=CARTESIAN_POINT('Ctrl Pts',(2.08166817117217E-16,3.,9.2));
#22070=CARTESIAN_POINT('Ctrl Pts',(0.251982495387347,3.,9.2));
#22071=CARTESIAN_POINT('Ctrl Pts',(0.520217657456258,3.05052306683097,9.18860399767844));
#22072=CARTESIAN_POINT('Ctrl Pts',(1.0127456170646,3.25488309906895,9.1474267505225));
#22073=CARTESIAN_POINT('Ctrl Pts',(1.23710338548845,3.40867626074226,9.11820719093608));
#22074=CARTESIAN_POINT('Ctrl Pts',(1.59133769071451,3.76291056596832,9.06309972244743));
#22075=CARTESIAN_POINT('Ctrl Pts',(1.7451199392152,3.98726244660274,9.0335726503792));
#22076=CARTESIAN_POINT('Ctrl Pts',(1.94947204040866,4.479769809412,8.99168712872246));
#22077=CARTESIAN_POINT('Ctrl Pts',(2.,4.74799765525699,8.97997772825746));
#22078=CARTESIAN_POINT('Ctrl Pts',(2.,5.,8.97997772825746));
#22079=CARTESIAN_POINT('Ctrl Pts',(2.,5.25200234474301,8.97997772825746));
#22080=CARTESIAN_POINT('Ctrl Pts',(1.94947204040866,5.520230190588,8.99168712872246));
#22081=CARTESIAN_POINT('Ctrl Pts',(1.7451199392152,6.01273755339726,9.0335726503792));
#22082=CARTESIAN_POINT('Ctrl Pts',(1.59133769071451,6.23708943403168,9.06309972244743));
#22083=CARTESIAN_POINT('Ctrl Pts',(1.23710338548845,6.59132373925774,9.11820719093608));
#22084=CARTESIAN_POINT('Ctrl Pts',(1.0127456170646,6.74511690093105,9.1474267505225));
#22085=CARTESIAN_POINT('Ctrl Pts',(0.520217657456256,6.94947693316903,9.18860399767844));
#22086=CARTESIAN_POINT('Ctrl Pts',(0.251982495387346,7.,9.2));
#22087=CARTESIAN_POINT('Ctrl Pts',(-0.251982495387347,7.,9.2));
#22088=CARTESIAN_POINT('Ctrl Pts',(-0.520217657456257,6.94947693316903,
9.18860399767844));
#22089=CARTESIAN_POINT('Ctrl Pts',(-1.0127456170646,6.74511690093105,9.1474267505225));
#22090=CARTESIAN_POINT('Ctrl Pts',(-1.23710338548845,6.59132373925774,9.11820719093608));
#22091=CARTESIAN_POINT('Ctrl Pts',(-1.59133769071452,6.23708943403168,9.06309972244743));
#22092=CARTESIAN_POINT('Ctrl Pts',(-1.7451199392152,6.01273755339726,9.0335726503792));
#22093=CARTESIAN_POINT('Ctrl Pts',(-1.94947204040866,5.520230190588,8.99168712872246));
#22094=CARTESIAN_POINT('Ctrl Pts',(-2.,5.25200234474301,8.97997772825746));
#22095=CARTESIAN_POINT('Ctrl Pts',(-2.,5.,8.97997772825746));
#22096=CARTESIAN_POINT('Ctrl Pts',(-2.,5.,8.97997772825746));
#22097=CARTESIAN_POINT('Ctrl Pts',(-2.,4.74799765525699,8.97997772825746));
#22098=CARTESIAN_POINT('Ctrl Pts',(-1.94947204040866,4.479769809412,8.99168712872246));
#22099=CARTESIAN_POINT('Ctrl Pts',(-1.7451199392152,3.98726244660274,9.0335726503792));
#22100=CARTESIAN_POINT('Ctrl Pts',(-1.59133769071452,3.76291056596832,9.06309972244743));
#22101=CARTESIAN_POINT('Ctrl Pts',(-1.23710338548845,3.40867626074226,9.11820719093608));
#22102=CARTESIAN_POINT('Ctrl Pts',(-1.0127456170646,3.25488309906895,9.1474267505225));
#22103=CARTESIAN_POINT('Ctrl Pts',(-0.520217657456257,3.05052306683097,
9.18860399767844));
#22104=CARTESIAN_POINT('Ctrl Pts',(-0.251982495387346,3.,9.2));
#22105=CARTESIAN_POINT('Ctrl Pts',(1.38777878078145E-16,3.,9.2));
#22106=CARTESIAN_POINT('',(0.,261.7,9.2));
#22107=CARTESIAN_POINT('',(-3.09999999999999,264.8,8.66198591548151));
#22108=CARTESIAN_POINT('Ctrl Pts',(6.93889390390723E-17,261.7,9.2));
#22109=CARTESIAN_POINT('Ctrl Pts',(0.392492181867812,261.7,9.2));
#22110=CARTESIAN_POINT('Ctrl Pts',(0.809098032285487,261.779064419326,9.17242354783845));
#22111=CARTESIAN_POINT('Ctrl Pts',(1.57202652449705,262.096405395141,9.07285654990429));
#22112=CARTESIAN_POINT('Ctrl Pts',(1.91858114764766,262.334519104291,9.00212872931236));
#22113=CARTESIAN_POINT('Ctrl Pts',(2.46561371815086,262.881551674794,8.86792542274352));
#22114=CARTESIAN_POINT('Ctrl Pts',(2.70362524494473,263.228053521236,8.79535506867642));
#22115=CARTESIAN_POINT('Ctrl Pts',(3.02088992440016,263.990785821449,8.69149502149013));
#22116=CARTESIAN_POINT('Ctrl Pts',(3.09999999999999,264.407317173429,8.66198591548151));
#22117=CARTESIAN_POINT('Ctrl Pts',(3.09999999999999,264.8,8.66198591548151));
#22118=CARTESIAN_POINT('Ctrl Pts',(3.09999999999999,265.192682826571,8.66198591548151));
#22119=CARTESIAN_POINT('Ctrl Pts',(3.02088992440016,265.609214178551,8.69149502149012));
#22120=CARTESIAN_POINT('Ctrl Pts',(2.70362524494473,266.371946478764,8.79535506867642));
#22121=CARTESIAN_POINT('Ctrl Pts',(2.46561371815086,266.718448325206,8.86792542274352));
#22122=CARTESIAN_POINT('Ctrl Pts',(1.91858114764766,267.265480895709,9.00212872931236));
#22123=CARTESIAN_POINT('Ctrl Pts',(1.57202652449705,267.503594604859,9.07285654990429));
#22124=CARTESIAN_POINT('Ctrl Pts',(0.809098032285487,267.820935580675,9.17242354783845));
#22125=CARTESIAN_POINT('Ctrl Pts',(0.392492181867812,267.9,9.2));
#22126=CARTESIAN_POINT('Ctrl Pts',(-0.392492181867813,267.9,9.2));
#22127=CARTESIAN_POINT('Ctrl Pts',(-0.809098032285488,267.820935580675,
9.17242354783845));
#22128=CARTESIAN_POINT('Ctrl Pts',(-1.57202652449705,267.503594604859,9.07285654990429));
#22129=CARTESIAN_POINT('Ctrl Pts',(-1.91858114764766,267.265480895709,9.00212872931236));
#22130=CARTESIAN_POINT('Ctrl Pts',(-2.46561371815086,266.718448325206,8.86792542274352));
#22131=CARTESIAN_POINT('Ctrl Pts',(-2.70362524494473,266.371946478764,8.79535506867642));
#22132=CARTESIAN_POINT('Ctrl Pts',(-3.02088992440016,265.609214178551,8.69149502149013));
#22133=CARTESIAN_POINT('Ctrl Pts',(-3.09999999999999,265.192682826571,8.66198591548151));
#22134=CARTESIAN_POINT('Ctrl Pts',(-3.09999999999999,264.8,8.66198591548151));
#22135=CARTESIAN_POINT('Ctrl Pts',(-3.09999999999999,264.8,8.66198591548151));
#22136=CARTESIAN_POINT('Ctrl Pts',(-3.09999999999999,264.407317173429,8.66198591548151));
#22137=CARTESIAN_POINT('Ctrl Pts',(-3.02088992440016,263.990785821449,8.69149502149012));
#22138=CARTESIAN_POINT('Ctrl Pts',(-2.70362524494473,263.228053521236,8.79535506867642));
#22139=CARTESIAN_POINT('Ctrl Pts',(-2.46561371815086,262.881551674794,8.86792542274352));
#22140=CARTESIAN_POINT('Ctrl Pts',(-1.91858114764766,262.334519104291,9.00212872931236));
#22141=CARTESIAN_POINT('Ctrl Pts',(-1.57202652449705,262.096405395141,9.07285654990429));
#22142=CARTESIAN_POINT('Ctrl Pts',(-0.809098032285487,261.779064419326,
9.17242354783845));
#22143=CARTESIAN_POINT('Ctrl Pts',(-0.392492181867816,261.7,9.2));
#22144=CARTESIAN_POINT('Ctrl Pts',(-4.09394740330526E-15,261.7,9.2));
#22145=CARTESIAN_POINT('Origin',(0.,264.8,-11.1));
#22146=CARTESIAN_POINT('',(-3.09999999999999,264.8,-11.1));
#22147=CARTESIAN_POINT('Origin',(0.,264.8,-11.1));
#22148=CARTESIAN_POINT('',(-3.09999999999999,264.8,-11.1));
#22149=CARTESIAN_POINT('Origin',(0.,5.,-11.1));
#22150=CARTESIAN_POINT('',(5.66553889764798E-16,7.,-10.6741648723787));
#22151=CARTESIAN_POINT('',(-2.,5.00000000004607,-10.4183332065073));
#22152=CARTESIAN_POINT('Ctrl Pts',(3.90311824664763E-16,7.,-10.6741648723787));
#22153=CARTESIAN_POINT('Ctrl Pts',(0.0905425845562135,7.,-10.67416643345));
#22154=CARTESIAN_POINT('Ctrl Pts',(0.180978358532567,6.99385302819578,-10.6726039986148));
#22155=CARTESIAN_POINT('Ctrl Pts',(0.522624030520656,6.94717907361443,-10.6609110333759));
#22156=CARTESIAN_POINT('Ctrl Pts',(0.764749077005449,6.86522985952275,-10.6402575275526));
#22157=CARTESIAN_POINT('Ctrl Pts',(1.21107417380008,6.61272549366747,-10.5843663956255));
#22158=CARTESIAN_POINT('Ctrl Pts',(1.41000159084709,6.44194367972254,-10.5494794983223));
#22159=CARTESIAN_POINT('Ctrl Pts',(1.7318707401912,6.03366519693967,-10.4846434012231));
#22160=CARTESIAN_POINT('Ctrl Pts',(1.85210598322984,5.79898238439151,-10.4555004640632));
#22161=CARTESIAN_POINT('Ctrl Pts',(1.9583401576163,5.42531015059408,-10.4290848493575));
#22162=CARTESIAN_POINT('Ctrl Pts',(1.98132978273519,5.30063336475968,-10.4231531964456));
#22163=CARTESIAN_POINT('Ctrl Pts',(2.00342374231953,5.0482782950185,-10.4174536861239));
#22164=CARTESIAN_POINT('Ctrl Pts',(2.00246887275993,4.92144779768745,-10.417702628372));
#22165=CARTESIAN_POINT('Ctrl Pts',(1.96358997015029,4.54336430699628,-10.4277230327553));
#22166=CARTESIAN_POINT('Ctrl Pts',(1.89017432113397,4.29951442558204,-10.4468643148236));
#22167=CARTESIAN_POINT('Ctrl Pts',(1.65371382249779,3.84551301214123,-10.5008923916095));
#22168=CARTESIAN_POINT('Ctrl Pts',(1.48992823087753,3.64081189954436,-10.5355071129865));
#22169=CARTESIAN_POINT('Ctrl Pts',(1.15765910613943,3.35964601502151,-10.5903139385164));
#22170=CARTESIAN_POINT('Ctrl Pts',(1.00877965860273,3.26405647735089,-10.6113011130337));
#22171=CARTESIAN_POINT('Ctrl Pts',(0.689508174816086,3.11436672263152,-10.645705448787));
#22172=CARTESIAN_POINT('Ctrl Pts',(0.52056030432242,3.06085078015626,-10.6589513899869));
#22173=CARTESIAN_POINT('Ctrl Pts',(0.346363582765798,3.03022024872484,-10.6665813564896));
#22174=CARTESIAN_POINT('Ctrl Pts',(0.222541532025453,3.00844753576438,-10.6720048690046));
#22175=CARTESIAN_POINT('Ctrl Pts',(0.096919746131382,2.99838937465003,-10.6745722719829));
#22176=CARTESIAN_POINT('Ctrl Pts',(-0.155712937316322,3.00204261420003,
-10.6736481591137));
#22177=CARTESIAN_POINT('Ctrl Pts',(-0.281945001971389,3.01593008051804,
-10.6701129134356));
#22178=CARTESIAN_POINT('Ctrl Pts',(-0.530158060286785,3.06737632605939,
-10.6573695392721));
#22179=CARTESIAN_POINT('Ctrl Pts',(-0.651515034820079,3.10486401462923,
-10.6481781924527));
#22180=CARTESIAN_POINT('Ctrl Pts',(-0.885673237124933,3.20229798323634,
-10.6253615082331));
#22181=CARTESIAN_POINT('Ctrl Pts',(-0.997931263074252,3.26212905175645,
-10.6117666796584));
#22182=CARTESIAN_POINT('Ctrl Pts',(-1.32191353329698,3.47649890889909,-10.5662536960044));
#22183=CARTESIAN_POINT('Ctrl Pts',(-1.50972131261701,3.66237708090707,-10.5305737460068));
#22184=CARTESIAN_POINT('Ctrl Pts',(-1.80282581791566,4.09551861849479,-10.4681951081463));
#22185=CARTESIAN_POINT('Ctrl Pts',(-1.90588825604454,4.33912828055132,-10.4422956738487));
#22186=CARTESIAN_POINT('Ctrl Pts',(-1.98631219662309,4.72977681278504,-10.4219160701683));
#22187=CARTESIAN_POINT('Ctrl Pts',(-2.00000000000623,4.86485757992022,-10.4183330488132));
#22188=CARTESIAN_POINT('Ctrl Pts',(-2.,5.00000000009213,-10.4183332065073));
#22189=CARTESIAN_POINT('',(-2.,5.,-11.1));
#22190=CARTESIAN_POINT('Ctrl Pts',(-2.,5.00000000009213,-10.4183332065073));
#22191=CARTESIAN_POINT('Ctrl Pts',(-1.99999999999466,5.11601901023085,-10.4183333418869));
#22192=CARTESIAN_POINT('Ctrl Pts',(-1.98991020136398,5.23208345991214,-10.4209668626609));
#22193=CARTESIAN_POINT('Ctrl Pts',(-1.92592478911155,5.59532890146743,-10.4372741617203));
#22194=CARTESIAN_POINT('Ctrl Pts',(-1.83579428369438,5.83229365962327,-10.4601816506442));
#22195=CARTESIAN_POINT('Ctrl Pts',(-1.56865648998154,6.26765940551044,-10.5187492985391));
#22196=CARTESIAN_POINT('Ctrl Pts',(-1.39075219046935,6.46059804253605,-10.5540922604607));
#22197=CARTESIAN_POINT('Ctrl Pts',(-1.07565913626136,6.69115396916685,-10.6015152323924));
#22198=CARTESIAN_POINT('Ctrl Pts',(-0.962845797709129,6.75786177513161,
-10.6163207779944));
#22199=CARTESIAN_POINT('Ctrl Pts',(-0.728007424527183,6.86719321021018,
-10.6414854333641));
#22200=CARTESIAN_POINT('Ctrl Pts',(-0.606894860616944,6.91001907374113,
-10.6518486458756));
#22201=CARTESIAN_POINT('Ctrl Pts',(-0.358236021802618,6.97180044684728,
-10.6670261603999));
#22202=CARTESIAN_POINT('Ctrl Pts',(-0.231503426306791,6.99067815064411,
-10.6718103168311));
#22203=CARTESIAN_POINT('Ctrl Pts',(-0.0690990145370653,6.99910518679761,
-10.6739387219855));
#22204=CARTESIAN_POINT('Ctrl Pts',(-0.0345417346423837,7.,-10.6741642768345));
#22205=CARTESIAN_POINT('Ctrl Pts',(3.0952483991701E-16,7.,-10.6741648723787));
#22206=CARTESIAN_POINT('Origin',(0.,5.,-11.1));
#22207=CARTESIAN_POINT('',(-2.,4.99999999999881,10.4183332085574));
#22208=CARTESIAN_POINT('',(-2.,5.,-11.1));
#22209=CARTESIAN_POINT('',(2.,5.,10.4183332061262));
#22210=CARTESIAN_POINT('Ctrl Pts',(-2.,4.99999999999762,10.4183332085574));
#22211=CARTESIAN_POINT('Ctrl Pts',(-1.99999999999971,4.75764050990674,10.4183333996923));
#22212=CARTESIAN_POINT('Ctrl Pts',(-1.95601203851425,4.51791095132192,10.4300808595327));
#22213=CARTESIAN_POINT('Ctrl Pts',(-1.78001439082704,4.05299932846605,10.4725856857188));
#22214=CARTESIAN_POINT('Ctrl Pts',(-1.64486906100864,3.83420865177878,10.5037554238368));
#22215=CARTESIAN_POINT('Ctrl Pts',(-1.29669691407628,3.45521458398486,10.5694095067776));
#22216=CARTESIAN_POINT('Ctrl Pts',(-1.08447711464625,3.29935703486476,10.6031801734129));
#22217=CARTESIAN_POINT('Ctrl Pts',(-0.614102032533418,3.07920133939685,
10.6537952714221));
#22218=CARTESIAN_POINT('Ctrl Pts',(-0.361056943994989,3.01584209266149,
10.6701647452922));
#22219=CARTESIAN_POINT('Ctrl Pts',(0.151263373348514,2.9896593782464,10.6767753112161));
#22220=CARTESIAN_POINT('Ctrl Pts',(0.40405218080261,3.0249721729091,10.667493673275));
#22221=CARTESIAN_POINT('Ctrl Pts',(0.887315218439553,3.18921348309502,10.6280783550302));
#22222=CARTESIAN_POINT('Ctrl Pts',(1.11205311096585,3.31806661278736,10.598173329718));
#22223=CARTESIAN_POINT('Ctrl Pts',(1.50518996696904,3.65702224569566,10.5326192482352));
#22224=CARTESIAN_POINT('Ctrl Pts',(1.66885927304681,3.86665024154239,10.4976296441678));
#22225=CARTESIAN_POINT('Ctrl Pts',(1.84524281816655,4.21783738115516,10.4570160383264));
#22226=CARTESIAN_POINT('Ctrl Pts',(1.89199289101732,4.33881643265941,10.4455972008102));
#22227=CARTESIAN_POINT('Ctrl Pts',(1.97544365595881,4.63862060372576,10.4248069793727));
#22228=CARTESIAN_POINT('Ctrl Pts',(2.,4.81896546073527,10.4183332250375));
#22229=CARTESIAN_POINT('Ctrl Pts',(2.,5.,10.4183332061262));
#22230=CARTESIAN_POINT('Ctrl Pts',(2.,5.,10.4183332061262));
#22231=CARTESIAN_POINT('Ctrl Pts',(2.,5.07412445802377,10.418333198383));
#22232=CARTESIAN_POINT('Ctrl Pts',(1.99588006958343,5.14836454540958,10.419403803429));
#22233=CARTESIAN_POINT('Ctrl Pts',(1.97348611150443,5.34850362220855,10.4251649570087));
#22234=CARTESIAN_POINT('Ctrl Pts',(1.94744895610822,5.47275424065624,10.4318462442253));
#22235=CARTESIAN_POINT('Ctrl Pts',(1.87218782309222,5.7148378129423,10.4504277671373));
#22236=CARTESIAN_POINT('Ctrl Pts',(1.82319167245477,5.83183046398235,10.4622438955467));
#22237=CARTESIAN_POINT('Ctrl Pts',(1.64087140867284,6.17270872224318,10.5036508546895));
#22238=CARTESIAN_POINT('Ctrl Pts',(1.47469697164074,6.37574114434066,10.5384558490889));
#22239=CARTESIAN_POINT('Ctrl Pts',(1.22410831831214,6.58299080923761,10.5792185726714));
#22240=CARTESIAN_POINT('Ctrl Pts',(1.17151858524451,6.62229933469441,10.5872695267222));
#22241=CARTESIAN_POINT('Ctrl Pts',(1.00965163715467,6.73129131268717,10.6103041534442));
#22242=CARTESIAN_POINT('Ctrl Pts',(0.895447882346682,6.79304313854791,10.6242895223643));
#22243=CARTESIAN_POINT('Ctrl Pts',(0.657087920935124,6.89336884418513,10.6477466535023));
#22244=CARTESIAN_POINT('Ctrl Pts',(0.533548659590622,6.93184892211207,10.6571764889425));
#22245=CARTESIAN_POINT('Ctrl Pts',(0.157607534485302,7.00998184253995,10.6765326365133));
#22246=CARTESIAN_POINT('Ctrl Pts',(-0.0990741273170037,7.01373005525968,
10.677526398444));
#22247=CARTESIAN_POINT('Ctrl Pts',(-0.475136684057559,6.94689825343089,
10.6608827373417));
#22248=CARTESIAN_POINT('Ctrl Pts',(-0.597744082024631,6.91279020306442,
10.65245495717));
#22249=CARTESIAN_POINT('Ctrl Pts',(-0.834479354355938,6.8220104651307,10.6309662827231));
#22250=CARTESIAN_POINT('Ctrl Pts',(-0.948120173018753,6.76552135149282,
10.6179467410782));
#22251=CARTESIAN_POINT('Ctrl Pts',(-1.27766645441521,6.56075349650328,10.5736998888191));
#22252=CARTESIAN_POINT('Ctrl Pts',(-1.4704451602617,6.38058619310992,10.5381856353254));
#22253=CARTESIAN_POINT('Ctrl Pts',(-1.7410164018396,6.00479346392452,10.4817961217748));
#22254=CARTESIAN_POINT('Ctrl Pts',(-1.83374938940646,5.82370479851062,10.4597876312556));
#22255=CARTESIAN_POINT('Ctrl Pts',(-1.9617280423452,5.43897136051534,10.4284252760763));
#22256=CARTESIAN_POINT('Ctrl Pts',(-1.99618860231403,5.2378760573922,10.4193156447857));
#22257=CARTESIAN_POINT('Ctrl Pts',(-1.99970195790469,5.03455443435168,10.4184105149837));
#22258=CARTESIAN_POINT('Ctrl Pts',(-1.99990107789324,5.02303114893203,10.4183592166078));
#22259=CARTESIAN_POINT('Ctrl Pts',(-2.00000000000001,5.0115126072,10.4183331994781));
#22260=CARTESIAN_POINT('Ctrl Pts',(-2.,4.99999999999762,10.4183332085574));
#22261=CARTESIAN_POINT('Origin',(0.,13.2,0.));
#22262=CARTESIAN_POINT('Origin',(-1.39303573403011E-15,13.2,11.375));
#22263=CARTESIAN_POINT('Origin',(0.,76.2,0.));
#22264=CARTESIAN_POINT('Origin',(-1.39303573403011E-15,76.2,11.375));
#22265=CARTESIAN_POINT('Ctrl Pts',(0.,32.7351420011818,-14.8300672611831));
#22266=CARTESIAN_POINT('Ctrl Pts',(0.,33.045415593,-14.3047121186603));
#22267=CARTESIAN_POINT('Ctrl Pts',(0.,33.63686551036,-13.97));
#22268=CARTESIAN_POINT('Ctrl Pts',(0.,34.2419663837872,-13.97));
#22269=CARTESIAN_POINT('Ctrl Pts',(3.73,32.7351420011818,-14.8300672611831));
#22270=CARTESIAN_POINT('Ctrl Pts',(3.73,33.045415593,-14.3047121186603));
#22271=CARTESIAN_POINT('Ctrl Pts',(3.73,33.63686551036,-13.97));
#22272=CARTESIAN_POINT('Ctrl Pts',(3.73,34.2419663837872,-13.97));
#22273=CARTESIAN_POINT('Ctrl Pts',(3.73,32.7351420011818,-11.1000672611831));
#22274=CARTESIAN_POINT('Ctrl Pts',(3.73,33.045415593,-10.5747121186603));
#22275=CARTESIAN_POINT('Ctrl Pts',(3.73,33.63686551036,-10.24));
#22276=CARTESIAN_POINT('Ctrl Pts',(3.73,34.2419663837872,-10.24));
#22277=CARTESIAN_POINT('Ctrl Pts',(2.28396628040981E-16,32.7351420011818,
-11.1000672611831));
#22278=CARTESIAN_POINT('Ctrl Pts',(2.28396628040981E-16,33.045415593,-10.5747121186603));
#22279=CARTESIAN_POINT('Ctrl Pts',(2.28396628040981E-16,33.63686551036,
-10.24));
#22280=CARTESIAN_POINT('Ctrl Pts',(2.28396628040981E-16,34.2419663837872,
-10.24));
#22281=CARTESIAN_POINT('Ctrl Pts',(-3.73,32.7351420011818,-11.1000672611831));
#22282=CARTESIAN_POINT('Ctrl Pts',(-3.73,33.045415593,-10.5747121186603));
#22283=CARTESIAN_POINT('Ctrl Pts',(-3.73,33.63686551036,-10.24));
#22284=CARTESIAN_POINT('Ctrl Pts',(-3.73,34.2419663837872,-10.24));
#22285=CARTESIAN_POINT('Ctrl Pts',(-3.73,32.7351420011818,-14.8300672611831));
#22286=CARTESIAN_POINT('Ctrl Pts',(-3.73,33.045415593,-14.3047121186603));
#22287=CARTESIAN_POINT('Ctrl Pts',(-3.73,33.63686551036,-13.97));
#22288=CARTESIAN_POINT('Ctrl Pts',(-3.73,34.2419663837872,-13.97));
#22289=CARTESIAN_POINT('Ctrl Pts',(0.,32.7351420011818,-14.8300672611831));
#22290=CARTESIAN_POINT('Ctrl Pts',(0.,33.045415593,-14.3047121186603));
#22291=CARTESIAN_POINT('Ctrl Pts',(0.,33.63686551036,-13.97));
#22292=CARTESIAN_POINT('Ctrl Pts',(0.,34.2419663837872,-13.97));
#22293=CARTESIAN_POINT('Origin',(0.,34.2419663837872,-12.105));
#22294=CARTESIAN_POINT('Origin',(0.,34.2419663837872,-12.105));
#22295=CARTESIAN_POINT('Origin',(0.,71.2419663837872,-12.105));
#22296=CARTESIAN_POINT('Ctrl Pts',(0.,71.2419663837872,-13.97));
#22297=CARTESIAN_POINT('Ctrl Pts',(0.,71.847073728999,-13.97));
#22298=CARTESIAN_POINT('Ctrl Pts',(0.,72.4385298261441,-14.3047192784616));
#22299=CARTESIAN_POINT('Ctrl Pts',(0.,72.7488007217793,-14.8300841178694));
#22300=CARTESIAN_POINT('Ctrl Pts',(3.73,71.2419663837872,-13.97));
#22301=CARTESIAN_POINT('Ctrl Pts',(3.73,71.847073728999,-13.97));
#22302=CARTESIAN_POINT('Ctrl Pts',(3.73,72.4385298261441,-14.3047192784616));
#22303=CARTESIAN_POINT('Ctrl Pts',(3.73,72.7488007217793,-14.8300841178694));
#22304=CARTESIAN_POINT('Ctrl Pts',(3.73,71.2419663837872,-10.24));
#22305=CARTESIAN_POINT('Ctrl Pts',(3.73,71.847073728999,-10.24));
#22306=CARTESIAN_POINT('Ctrl Pts',(3.73,72.4385298261441,-10.5747192784616));
#22307=CARTESIAN_POINT('Ctrl Pts',(3.73,72.7488007217793,-11.1000841178694));
#22308=CARTESIAN_POINT('Ctrl Pts',(2.28396628040981E-16,71.2419663837872,
-10.24));
#22309=CARTESIAN_POINT('Ctrl Pts',(2.28396628040981E-16,71.847073728999,
-10.24));
#22310=CARTESIAN_POINT('Ctrl Pts',(2.28396628040981E-16,72.4385298261441,
-10.5747192784616));
#22311=CARTESIAN_POINT('Ctrl Pts',(2.28396628040981E-16,72.7488007217793,
-11.1000841178694));
#22312=CARTESIAN_POINT('Ctrl Pts',(-3.73,71.2419663837872,-10.24));
#22313=CARTESIAN_POINT('Ctrl Pts',(-3.73,71.847073728999,-10.24));
#22314=CARTESIAN_POINT('Ctrl Pts',(-3.73,72.4385298261441,-10.5747192784616));
#22315=CARTESIAN_POINT('Ctrl Pts',(-3.73,72.7488007217793,-11.1000841178694));
#22316=CARTESIAN_POINT('Ctrl Pts',(-3.73,71.2419663837872,-13.97));
#22317=CARTESIAN_POINT('Ctrl Pts',(-3.73,71.847073728999,-13.97));
#22318=CARTESIAN_POINT('Ctrl Pts',(-3.73,72.4385298261441,-14.3047192784616));
#22319=CARTESIAN_POINT('Ctrl Pts',(-3.73,72.7488007217793,-14.8300841178694));
#22320=CARTESIAN_POINT('Ctrl Pts',(0.,71.2419663837872,-13.97));
#22321=CARTESIAN_POINT('Ctrl Pts',(0.,71.847073728999,-13.97));
#22322=CARTESIAN_POINT('Ctrl Pts',(0.,72.4385298261441,-14.3047192784616));
#22323=CARTESIAN_POINT('Ctrl Pts',(0.,72.7488007217793,-14.8300841178694));
#22324=CARTESIAN_POINT('Ctrl Pts',(8.71689482662887,32.7351420011818,-11.9977764420207));
#22325=CARTESIAN_POINT('Ctrl Pts',(8.40809882163646,33.045415593,-11.5727552036368));
#22326=CARTESIAN_POINT('Ctrl Pts',(8.21135997452586,33.63686551036,-11.301967411418));
#22327=CARTESIAN_POINT('Ctrl Pts',(8.21135997452587,34.2419663837872,-11.301967411418));
#22328=CARTESIAN_POINT('Ctrl Pts',(11.7345282156474,32.7351420011818,-9.80533745096972));
#22329=CARTESIAN_POINT('Ctrl Pts',(11.4257322106545,33.045415593,-9.38031621258584));
#22330=CARTESIAN_POINT('Ctrl Pts',(11.2289933635444,33.63686551036,-9.10952842036708));
#22331=CARTESIAN_POINT('Ctrl Pts',(11.2289933635444,34.2419663837872,-9.10952842036708));
#22332=CARTESIAN_POINT('Ctrl Pts',(9.54208922459649,32.7351420011818,-6.78770406195117));
#22333=CARTESIAN_POINT('Ctrl Pts',(9.23329321960567,33.045415593,-6.36268282356729));
#22334=CARTESIAN_POINT('Ctrl Pts',(9.03655437249349,33.63686551036,-6.09189503134852));
#22335=CARTESIAN_POINT('Ctrl Pts',(9.03655437249349,34.2419663837872,-6.09189503134852));
#22336=CARTESIAN_POINT('Ctrl Pts',(6.52445583557794,32.7351420011818,-8.9801430530021));
#22337=CARTESIAN_POINT('Ctrl Pts',(6.21565983058659,33.045415593,-8.55512181461823));
#22338=CARTESIAN_POINT('Ctrl Pts',(6.01892098347494,33.63686551036,-8.28433402239945));
#22339=CARTESIAN_POINT('Ctrl Pts',(6.01892098347494,34.2419663837872,-8.28433402239945));
#22340=CARTESIAN_POINT('Ctrl Pts',(3.50682244655939,32.7351420011818,-11.172582044053));
#22341=CARTESIAN_POINT('Ctrl Pts',(3.19802644156751,33.045415593,-10.7475608056691));
#22342=CARTESIAN_POINT('Ctrl Pts',(3.00128759445638,33.63686551036,-10.4767730134504));
#22343=CARTESIAN_POINT('Ctrl Pts',(3.00128759445639,34.2419663837872,-10.4767730134504));
#22344=CARTESIAN_POINT('Ctrl Pts',(5.69926143761032,32.7351420011818,-14.1902154330716));
#22345=CARTESIAN_POINT('Ctrl Pts',(5.39046543261844,33.045415593,-13.7651941946877));
#22346=CARTESIAN_POINT('Ctrl Pts',(5.19372658550731,33.63686551036,-13.4944064024689));
#22347=CARTESIAN_POINT('Ctrl Pts',(5.19372658550731,34.2419663837872,-13.4944064024689));
#22348=CARTESIAN_POINT('Ctrl Pts',(8.71689482662887,32.7351420011818,-11.9977764420207));
#22349=CARTESIAN_POINT('Ctrl Pts',(8.40809882163646,33.045415593,-11.5727552036368));
#22350=CARTESIAN_POINT('Ctrl Pts',(8.21135997452586,33.63686551036,-11.301967411418));
#22351=CARTESIAN_POINT('Ctrl Pts',(8.21135997452587,34.2419663837872,-11.301967411418));
#22352=CARTESIAN_POINT('Origin',(7.1151404790004,34.2419663837872,-9.79315071690873));
#22353=CARTESIAN_POINT('Origin',(7.1151404790004,34.2419663837872,-9.79315071690873));
#22354=CARTESIAN_POINT('Origin',(7.1151404790004,71.2419663837872,-9.79315071690873));
#22355=CARTESIAN_POINT('Ctrl Pts',(8.21135997452587,71.2419663837872,-11.301967411418));
#22356=CARTESIAN_POINT('Ctrl Pts',(8.21135997452587,71.847073728999,-11.301967411418));
#22357=CARTESIAN_POINT('Ctrl Pts',(8.40810303006151,72.4385298261441,-11.572760996038));
#22358=CARTESIAN_POINT('Ctrl Pts',(8.71690473474048,72.7488007217793,-11.9977900793663));
#22359=CARTESIAN_POINT('Ctrl Pts',(11.2289933635444,71.2419663837872,-9.10952842036708));
#22360=CARTESIAN_POINT('Ctrl Pts',(11.2289933635444,71.847073728999,-9.10952842036708));
#22361=CARTESIAN_POINT('Ctrl Pts',(11.4257364190791,72.4385298261441,-9.38032200498704));
#22362=CARTESIAN_POINT('Ctrl Pts',(11.734538123759,72.7488007217793,-9.8053510883154));
#22363=CARTESIAN_POINT('Ctrl Pts',(9.03655437249349,71.2419663837872,-6.09189503134853));
#22364=CARTESIAN_POINT('Ctrl Pts',(9.03655437249349,71.847073728999,-6.09189503134853));
#22365=CARTESIAN_POINT('Ctrl Pts',(9.23329742803191,72.4385298261441,-6.36268861596848));
#22366=CARTESIAN_POINT('Ctrl Pts',(9.5420991327081,72.7488007217793,-6.78771769929685));
#22367=CARTESIAN_POINT('Ctrl Pts',(6.01892098347494,71.2419663837872,-8.28433402239945));
#22368=CARTESIAN_POINT('Ctrl Pts',(6.01892098347494,71.847073728999,-8.28433402239945));
#22369=CARTESIAN_POINT('Ctrl Pts',(6.21566403901243,72.4385298261441,-8.55512760701941));
#22370=CARTESIAN_POINT('Ctrl Pts',(6.52446574368955,72.7488007217793,-8.98015669034778));
#22371=CARTESIAN_POINT('Ctrl Pts',(3.00128759445639,71.2419663837872,-10.4767730134504));
#22372=CARTESIAN_POINT('Ctrl Pts',(3.00128759445639,71.847073728999,-10.4767730134504));
#22373=CARTESIAN_POINT('Ctrl Pts',(3.19803064999295,72.4385298261441,-10.7475665980703));
#22374=CARTESIAN_POINT('Ctrl Pts',(3.506832354671,72.7488007217793,-11.1725956813987));
#22375=CARTESIAN_POINT('Ctrl Pts',(5.19372658550732,71.2419663837872,-13.4944064024689));
#22376=CARTESIAN_POINT('Ctrl Pts',(5.19372658550732,71.847073728999,-13.4944064024689));
#22377=CARTESIAN_POINT('Ctrl Pts',(5.39046964104388,72.4385298261441,-13.7651999870889));
#22378=CARTESIAN_POINT('Ctrl Pts',(5.69927134572193,72.7488007217793,-14.1902290704173));
#22379=CARTESIAN_POINT('Ctrl Pts',(8.21135997452587,71.2419663837872,-11.301967411418));
#22380=CARTESIAN_POINT('Ctrl Pts',(8.21135997452587,71.847073728999,-11.301967411418));
#22381=CARTESIAN_POINT('Ctrl Pts',(8.40810303006151,72.4385298261441,-11.572760996038));
#22382=CARTESIAN_POINT('Ctrl Pts',(8.71690473474048,72.7488007217793,-11.9977900793663));
#22383=CARTESIAN_POINT('Ctrl Pts',(14.1042321058436,32.7351420011818,-4.58274281142907));
#22384=CARTESIAN_POINT('Ctrl Pts',(13.604589674176,33.045415593,-4.42039914430687));
#22385=CARTESIAN_POINT('Ctrl Pts',(13.2862595326433,33.63686551036,-4.31696741141798));
#22386=CARTESIAN_POINT('Ctrl Pts',(13.2862595326433,34.2419663837872,-4.31696741141798));
#22387=CARTESIAN_POINT('Ctrl Pts',(15.2568654948622,32.7351420011818,-1.03530200564814));
#22388=CARTESIAN_POINT('Ctrl Pts',(14.7572230631946,33.045415593,-0.872958338525147));
#22389=CARTESIAN_POINT('Ctrl Pts',(14.4388929216619,33.63686551036,-0.76952660563705));
#22390=CARTESIAN_POINT('Ctrl Pts',(14.4388929216619,34.2419663837872,-0.769526605637051));
#22391=CARTESIAN_POINT('Ctrl Pts',(11.7094246890812,32.7351420011818,0.117331383370402));
#22392=CARTESIAN_POINT('Ctrl Pts',(11.2097822574136,33.045415593,0.279675050492603));
#22393=CARTESIAN_POINT('Ctrl Pts',(10.8914521158809,33.63686551036,0.383106783381494));
#22394=CARTESIAN_POINT('Ctrl Pts',(10.8914521158809,34.2419663837872,0.383106783381493));
#22395=CARTESIAN_POINT('Ctrl Pts',(10.5567913000627,32.7351420011818,-3.43010942241053));
#22396=CARTESIAN_POINT('Ctrl Pts',(10.0571488683951,33.045415593,-3.26776575528832));
#22397=CARTESIAN_POINT('Ctrl Pts',(9.73881872686238,33.63686551036,-3.16433402239943));
#22398=CARTESIAN_POINT('Ctrl Pts',(9.73881872686238,34.2419663837872,-3.16433402239943));
#22399=CARTESIAN_POINT('Ctrl Pts',(9.40415791104414,32.7351420011818,-6.97755022819145));
#22400=CARTESIAN_POINT('Ctrl Pts',(8.90451547937655,33.045415593,-6.81520656106925));
#22401=CARTESIAN_POINT('Ctrl Pts',(8.58618533784384,33.63686551036,-6.71177482818036));
#22402=CARTESIAN_POINT('Ctrl Pts',(8.58618533784384,34.2419663837872,-6.71177482818036));
#22403=CARTESIAN_POINT('Ctrl Pts',(12.9515987168251,32.7351420011818,-8.13018361720999));
#22404=CARTESIAN_POINT('Ctrl Pts',(12.4519562851575,33.045415593,-7.96783995008859));
#22405=CARTESIAN_POINT('Ctrl Pts',(12.1336261436248,33.63686551036,-7.86440821719891));
#22406=CARTESIAN_POINT('Ctrl Pts',(12.1336261436248,34.2419663837872,-7.86440821719891));
#22407=CARTESIAN_POINT('Ctrl Pts',(14.1042321058436,32.7351420011818,-4.58274281142907));
#22408=CARTESIAN_POINT('Ctrl Pts',(13.604589674176,33.045415593,-4.42039914430687));
#22409=CARTESIAN_POINT('Ctrl Pts',(13.2862595326433,33.63686551036,-4.31696741141798));
#22410=CARTESIAN_POINT('Ctrl Pts',(13.2862595326433,34.2419663837872,-4.31696741141798));
#22411=CARTESIAN_POINT('Origin',(11.5125391297528,34.2419663837872,-3.74065071690871));
#22412=CARTESIAN_POINT('Origin',(11.5125391297528,34.2419663837872,-3.74065071690871));
#22413=CARTESIAN_POINT('Origin',(11.5125391297528,71.2419663837872,-3.74065071690871));
#22414=CARTESIAN_POINT('Ctrl Pts',(13.2862595326433,71.2419663837872,-4.31696741141798));
#22415=CARTESIAN_POINT('Ctrl Pts',(13.2862595326433,71.847073728999,-4.31696741141798));
#22416=CARTESIAN_POINT('Ctrl Pts',(13.6045964835519,72.4385298261441,-4.42040135680742));
#22417=CARTESIAN_POINT('Ctrl Pts',(14.104248137505,72.7488007217793,-4.5827480204316));
#22418=CARTESIAN_POINT('Ctrl Pts',(14.4388929216619,71.2419663837872,-0.769526605637053));
#22419=CARTESIAN_POINT('Ctrl Pts',(14.4388929216619,71.847073728999,-0.769526605637052));
#22420=CARTESIAN_POINT('Ctrl Pts',(14.7572298725705,72.4385298261441,-0.872960551026562));
#22421=CARTESIAN_POINT('Ctrl Pts',(15.2568815265235,72.7488007217793,-1.03530721465068));
#22422=CARTESIAN_POINT('Ctrl Pts',(10.8914521158809,71.2419663837872,0.383106783381491));
#22423=CARTESIAN_POINT('Ctrl Pts',(10.8914521158809,71.847073728999,0.383106783381492));
#22424=CARTESIAN_POINT('Ctrl Pts',(11.2097890667895,72.4385298261441,0.279672837992247));
#22425=CARTESIAN_POINT('Ctrl Pts',(11.7094407207426,72.7488007217793,0.117326174367868));
#22426=CARTESIAN_POINT('Ctrl Pts',(9.73881872686238,71.2419663837872,-3.16433402239944));
#22427=CARTESIAN_POINT('Ctrl Pts',(9.73881872686238,71.847073728999,-3.16433402239943));
#22428=CARTESIAN_POINT('Ctrl Pts',(10.057155677771,72.4385298261441,-3.26776796778875));
#22429=CARTESIAN_POINT('Ctrl Pts',(10.556807331724,72.7488007217793,-3.43011463141306));
#22430=CARTESIAN_POINT('Ctrl Pts',(8.58618533784384,71.2419663837872,-6.71177482818036));
#22431=CARTESIAN_POINT('Ctrl Pts',(8.58618533784384,71.847073728999,-6.71177482818036));
#22432=CARTESIAN_POINT('Ctrl Pts',(8.90452228875243,72.4385298261441,-6.81520877356974));
#22433=CARTESIAN_POINT('Ctrl Pts',(9.40417394270549,72.7488007217793,-6.97755543719399));
#22434=CARTESIAN_POINT('Ctrl Pts',(12.1336261436248,71.2419663837872,-7.86440821719891));
#22435=CARTESIAN_POINT('Ctrl Pts',(12.1336261436248,71.847073728999,-7.86440821719891));
#22436=CARTESIAN_POINT('Ctrl Pts',(12.4519630945334,72.4385298261441,-7.96784216258828));
#22437=CARTESIAN_POINT('Ctrl Pts',(12.9516147484864,72.7488007217793,-8.13018882621253));
#22438=CARTESIAN_POINT('Ctrl Pts',(13.2862595326433,71.2419663837872,-4.31696741141798));
#22439=CARTESIAN_POINT('Ctrl Pts',(13.2862595326433,71.847073728999,-4.31696741141798));
#22440=CARTESIAN_POINT('Ctrl Pts',(13.6045964835519,72.4385298261441,-4.42040135680742));
#22441=CARTESIAN_POINT('Ctrl Pts',(14.104248137505,72.7488007217793,-4.5827480204316));
#22442=CARTESIAN_POINT('Ctrl Pts',(14.1042321058436,32.7351420011818,4.58274281142917));
#22443=CARTESIAN_POINT('Ctrl Pts',(13.604589674176,33.045415593,4.42039914430803));
#22444=CARTESIAN_POINT('Ctrl Pts',(13.2862595326433,33.63686551036,4.31696741141807));
#22445=CARTESIAN_POINT('Ctrl Pts',(13.2862595326433,34.2419663837872,4.31696741141807));
#22446=CARTESIAN_POINT('Ctrl Pts',(12.951598716825,32.7351420011818,8.1301836172101));
#22447=CARTESIAN_POINT('Ctrl Pts',(12.4519562851574,33.045415593,7.96783995008948));
#22448=CARTESIAN_POINT('Ctrl Pts',(12.1336261436247,33.63686551036,7.86440821719899));
#22449=CARTESIAN_POINT('Ctrl Pts',(12.1336261436247,34.2419663837872,7.86440821719899));
#22450=CARTESIAN_POINT('Ctrl Pts',(9.40415791104411,32.7351420011818,6.97755022819152));
#22451=CARTESIAN_POINT('Ctrl Pts',(8.90451547937651,33.045415593,6.81520656107038));
#22452=CARTESIAN_POINT('Ctrl Pts',(8.58618533784379,33.63686551036,6.71177482818042));
#22453=CARTESIAN_POINT('Ctrl Pts',(8.58618533784379,34.2419663837872,6.71177482818042));
#22454=CARTESIAN_POINT('Ctrl Pts',(10.5567913000627,32.7351420011818,3.43010942241061));
#22455=CARTESIAN_POINT('Ctrl Pts',(10.0571488683951,33.045415593,3.26776575528946));
#22456=CARTESIAN_POINT('Ctrl Pts',(9.73881872686236,33.63686551036,3.1643340223995));
#22457=CARTESIAN_POINT('Ctrl Pts',(9.73881872686236,34.2419663837872,3.16433402239951));
#22458=CARTESIAN_POINT('Ctrl Pts',(11.7094246890812,32.7351420011818,-0.117331383370314));
#22459=CARTESIAN_POINT('Ctrl Pts',(11.2097822574137,33.045415593,-0.279675050491458));
#22460=CARTESIAN_POINT('Ctrl Pts',(10.8914521158809,33.63686551036,-0.383106783381414));
#22461=CARTESIAN_POINT('Ctrl Pts',(10.8914521158809,34.2419663837872,-0.383106783381413));
#22462=CARTESIAN_POINT('Ctrl Pts',(15.2568654948622,32.7351420011818,1.03530200564826));
#22463=CARTESIAN_POINT('Ctrl Pts',(14.7572230631946,33.045415593,0.872958338526582));
#22464=CARTESIAN_POINT('Ctrl Pts',(14.4388929216619,33.63686551036,0.769526605637155));
#22465=CARTESIAN_POINT('Ctrl Pts',(14.4388929216619,34.2419663837872,0.769526605637156));
#22466=CARTESIAN_POINT('Ctrl Pts',(14.1042321058436,32.7351420011818,4.58274281142917));
#22467=CARTESIAN_POINT('Ctrl Pts',(13.604589674176,33.045415593,4.42039914430803));
#22468=CARTESIAN_POINT('Ctrl Pts',(13.2862595326433,33.63686551036,4.31696741141807));
#22469=CARTESIAN_POINT('Ctrl Pts',(13.2862595326433,34.2419663837872,4.31696741141807));
#22470=CARTESIAN_POINT('Origin',(11.5125391297528,34.2419663837872,3.74065071690879));
#22471=CARTESIAN_POINT('Origin',(11.5125391297528,34.2419663837872,3.74065071690879));
#22472=CARTESIAN_POINT('Origin',(11.5125391297528,71.2419663837872,3.74065071690879));
#22473=CARTESIAN_POINT('Ctrl Pts',(13.2862595326433,71.2419663837872,4.31696741141807));
#22474=CARTESIAN_POINT('Ctrl Pts',(13.2862595326433,71.847073728999,4.31696741141807));
#22475=CARTESIAN_POINT('Ctrl Pts',(13.6045964835519,72.4385298261441,4.42040135680726));
#22476=CARTESIAN_POINT('Ctrl Pts',(14.1042481375049,72.7488007217793,4.58274802043171));
#22477=CARTESIAN_POINT('Ctrl Pts',(12.1336261436247,71.2419663837872,7.86440821719899));
#22478=CARTESIAN_POINT('Ctrl Pts',(12.1336261436247,71.847073728999,7.86440821719899));
#22479=CARTESIAN_POINT('Ctrl Pts',(12.4519630945333,72.4385298261441,7.96784216258811));
#22480=CARTESIAN_POINT('Ctrl Pts',(12.9516147484864,72.7488007217793,8.13018882621263));
#22481=CARTESIAN_POINT('Ctrl Pts',(8.58618533784379,71.2419663837872,6.71177482818042));
#22482=CARTESIAN_POINT('Ctrl Pts',(8.58618533784379,71.847073728999,6.71177482818042));
#22483=CARTESIAN_POINT('Ctrl Pts',(8.90452228875239,72.4385298261441,6.81520877356968));
#22484=CARTESIAN_POINT('Ctrl Pts',(9.40417394270545,72.7488007217793,6.97755543719405));
#22485=CARTESIAN_POINT('Ctrl Pts',(9.73881872686236,71.2419663837872,3.16433402239951));
#22486=CARTESIAN_POINT('Ctrl Pts',(9.73881872686236,71.847073728999,3.16433402239951));
#22487=CARTESIAN_POINT('Ctrl Pts',(10.057155677771,72.4385298261441,3.26776796778882));
#22488=CARTESIAN_POINT('Ctrl Pts',(10.556807331724,72.7488007217793,3.43011463141314));
#22489=CARTESIAN_POINT('Ctrl Pts',(10.8914521158809,71.2419663837872,-0.383106783381413));
#22490=CARTESIAN_POINT('Ctrl Pts',(10.8914521158809,71.847073728999,-0.383106783381413));
#22491=CARTESIAN_POINT('Ctrl Pts',(11.2097890667895,72.4385298261441,-0.27967283799203));
#22492=CARTESIAN_POINT('Ctrl Pts',(11.7094407207426,72.7488007217793,-0.117326174367781));
#22493=CARTESIAN_POINT('Ctrl Pts',(14.4388929216619,71.2419663837872,0.769526605637156));
#22494=CARTESIAN_POINT('Ctrl Pts',(14.4388929216619,71.847073728999,0.769526605637156));
#22495=CARTESIAN_POINT('Ctrl Pts',(14.7572298725704,72.4385298261441,0.872960551026407));
#22496=CARTESIAN_POINT('Ctrl Pts',(15.2568815265235,72.7488007217793,1.03530721465079));
#22497=CARTESIAN_POINT('Ctrl Pts',(13.2862595326433,71.2419663837872,4.31696741141807));
#22498=CARTESIAN_POINT('Ctrl Pts',(13.2862595326433,71.847073728999,4.31696741141807));
#22499=CARTESIAN_POINT('Ctrl Pts',(13.6045964835519,72.4385298261441,4.42040135680726));
#22500=CARTESIAN_POINT('Ctrl Pts',(14.1042481375049,72.7488007217793,4.58274802043171));
#22501=CARTESIAN_POINT('Ctrl Pts',(8.71689482662879,32.7351420011818,11.9977764420207));
#22502=CARTESIAN_POINT('Ctrl Pts',(8.40809882163849,33.045415593,11.5727552036368));
#22503=CARTESIAN_POINT('Ctrl Pts',(8.21135997452579,33.63686551036,11.3019674114181));
#22504=CARTESIAN_POINT('Ctrl Pts',(8.21135997452579,34.2419663837872,11.3019674114181));
#22505=CARTESIAN_POINT('Ctrl Pts',(5.69926143761022,32.7351420011818,14.1902154330716));
#22506=CARTESIAN_POINT('Ctrl Pts',(5.39046543261953,33.045415593,13.7651941946877));
#22507=CARTESIAN_POINT('Ctrl Pts',(5.19372658550722,33.63686551036,13.494406402469));
#22508=CARTESIAN_POINT('Ctrl Pts',(5.19372658550722,34.2419663837872,13.494406402469));
#22509=CARTESIAN_POINT('Ctrl Pts',(3.50682244655931,32.7351420011818,11.172582044053));
#22510=CARTESIAN_POINT('Ctrl Pts',(3.19802644156862,33.045415593,10.7475608056692));
#22511=CARTESIAN_POINT('Ctrl Pts',(3.00128759445631,33.63686551036,10.4767730134504));
#22512=CARTESIAN_POINT('Ctrl Pts',(3.00128759445631,34.2419663837872,10.4767730134504));
#22513=CARTESIAN_POINT('Ctrl Pts',(6.52445583557788,32.7351420011818,8.98014305300214));
#22514=CARTESIAN_POINT('Ctrl Pts',(6.21565983058679,33.045415593,8.55512181461826));
#22515=CARTESIAN_POINT('Ctrl Pts',(6.01892098347488,33.63686551036,8.28433402239949));
#22516=CARTESIAN_POINT('Ctrl Pts',(6.01892098347488,34.2419663837872,8.2843340223995));
#22517=CARTESIAN_POINT('Ctrl Pts',(9.54208922459645,32.7351420011818,6.78770406195123));
#22518=CARTESIAN_POINT('Ctrl Pts',(9.23329321960496,33.045415593,6.36268282356736));
#22519=CARTESIAN_POINT('Ctrl Pts',(9.03655437249344,33.63686551036,6.09189503134859));
#22520=CARTESIAN_POINT('Ctrl Pts',(9.03655437249345,34.2419663837872,6.09189503134859));
#22521=CARTESIAN_POINT('Ctrl Pts',(11.7345282156474,32.7351420011818,9.8053374509698));
#22522=CARTESIAN_POINT('Ctrl Pts',(11.4257322106575,33.045415593,9.38031621258592));
#22523=CARTESIAN_POINT('Ctrl Pts',(11.2289933635444,33.63686551036,9.10952842036716));
#22524=CARTESIAN_POINT('Ctrl Pts',(11.2289933635444,34.2419663837872,9.10952842036715));
#22525=CARTESIAN_POINT('Ctrl Pts',(8.71689482662879,32.7351420011818,11.9977764420207));
#22526=CARTESIAN_POINT('Ctrl Pts',(8.40809882163849,33.045415593,11.5727552036368));
#22527=CARTESIAN_POINT('Ctrl Pts',(8.21135997452579,33.63686551036,11.3019674114181));
#22528=CARTESIAN_POINT('Ctrl Pts',(8.21135997452579,34.2419663837872,11.3019674114181));
#22529=CARTESIAN_POINT('Origin',(7.11514047900033,34.2419663837872,9.79315071690878));
#22530=CARTESIAN_POINT('Origin',(7.11514047900033,34.2419663837872,9.79315071690878));
#22531=CARTESIAN_POINT('Origin',(7.11514047900033,71.2419663837872,9.79315071690878));
#22532=CARTESIAN_POINT('Ctrl Pts',(8.21135997452579,71.2419663837872,11.3019674114181));
#22533=CARTESIAN_POINT('Ctrl Pts',(8.21135997452579,71.847073728999,11.3019674114181));
#22534=CARTESIAN_POINT('Ctrl Pts',(8.40810303006512,72.4385298261441,11.572760996038));
#22535=CARTESIAN_POINT('Ctrl Pts',(8.7169047347404,72.7488007217793,11.9977900793664));
#22536=CARTESIAN_POINT('Ctrl Pts',(5.19372658550722,71.2419663837872,13.494406402469));
#22537=CARTESIAN_POINT('Ctrl Pts',(5.19372658550722,71.847073728999,13.494406402469));
#22538=CARTESIAN_POINT('Ctrl Pts',(5.39046964104563,72.4385298261441,13.7651999870889));
#22539=CARTESIAN_POINT('Ctrl Pts',(5.69927134572183,72.7488007217793,14.1902290704173));
#22540=CARTESIAN_POINT('Ctrl Pts',(3.00128759445631,71.2419663837872,10.4767730134504));
#22541=CARTESIAN_POINT('Ctrl Pts',(3.00128759445631,71.847073728999,10.4767730134504));
#22542=CARTESIAN_POINT('Ctrl Pts',(3.19803064999473,72.4385298261441,10.7475665980704));
#22543=CARTESIAN_POINT('Ctrl Pts',(3.50683235467092,72.7488007217793,11.1725956813987));
#22544=CARTESIAN_POINT('Ctrl Pts',(6.01892098347488,71.2419663837872,8.2843340223995));
#22545=CARTESIAN_POINT('Ctrl Pts',(6.01892098347488,71.847073728999,8.2843340223995));
#22546=CARTESIAN_POINT('Ctrl Pts',(6.21566403901237,72.4385298261441,8.55512760701946));
#22547=CARTESIAN_POINT('Ctrl Pts',(6.52446574368949,72.7488007217793,8.98015669034783));
#22548=CARTESIAN_POINT('Ctrl Pts',(9.03655437249345,71.2419663837872,6.09189503134859));
#22549=CARTESIAN_POINT('Ctrl Pts',(9.03655437249345,71.847073728999,6.09189503134859));
#22550=CARTESIAN_POINT('Ctrl Pts',(9.23329742803001,72.4385298261441,6.36268861596855));
#22551=CARTESIAN_POINT('Ctrl Pts',(9.54209913270805,72.7488007217793,6.78771769929692));
#22552=CARTESIAN_POINT('Ctrl Pts',(11.2289933635444,71.2419663837872,9.10952842036715));
#22553=CARTESIAN_POINT('Ctrl Pts',(11.2289933635444,71.847073728999,9.10952842036715));
#22554=CARTESIAN_POINT('Ctrl Pts',(11.4257364190846,72.4385298261441,9.38032200498712));
#22555=CARTESIAN_POINT('Ctrl Pts',(11.734538123759,72.7488007217793,9.80535108831548));
#22556=CARTESIAN_POINT('Ctrl Pts',(8.21135997452579,71.2419663837872,11.3019674114181));
#22557=CARTESIAN_POINT('Ctrl Pts',(8.21135997452579,71.847073728999,11.3019674114181));
#22558=CARTESIAN_POINT('Ctrl Pts',(8.40810303006512,72.4385298261441,11.572760996038));
#22559=CARTESIAN_POINT('Ctrl Pts',(8.7169047347404,72.7488007217793,11.9977900793664));
#22560=CARTESIAN_POINT('Ctrl Pts',(0.,32.7351420011818,14.8300672611831));
#22561=CARTESIAN_POINT('Ctrl Pts',(0.,33.045415593,14.3047121186603));
#22562=CARTESIAN_POINT('Ctrl Pts',(0.,33.63686551036,13.97));
#22563=CARTESIAN_POINT('Ctrl Pts',(0.,34.2419663837872,13.97));
#22564=CARTESIAN_POINT('Ctrl Pts',(-3.73,32.7351420011818,14.8300672611831));
#22565=CARTESIAN_POINT('Ctrl Pts',(-3.73,33.045415593,14.3047121186603));
#22566=CARTESIAN_POINT('Ctrl Pts',(-3.73,33.63686551036,13.97));
#22567=CARTESIAN_POINT('Ctrl Pts',(-3.73,34.2419663837872,13.97));
#22568=CARTESIAN_POINT('Ctrl Pts',(-3.73,32.7351420011818,11.1000672611831));
#22569=CARTESIAN_POINT('Ctrl Pts',(-3.73,33.045415593,10.5747121186603));
#22570=CARTESIAN_POINT('Ctrl Pts',(-3.73,33.63686551036,10.24));
#22571=CARTESIAN_POINT('Ctrl Pts',(-3.73,34.2419663837872,10.24));
#22572=CARTESIAN_POINT('Ctrl Pts',(-2.28396628040981E-16,32.7351420011818,
11.1000672611831));
#22573=CARTESIAN_POINT('Ctrl Pts',(-2.28396628040981E-16,33.045415593,10.5747121186603));
#22574=CARTESIAN_POINT('Ctrl Pts',(-2.28396628040981E-16,33.63686551036,
10.24));
#22575=CARTESIAN_POINT('Ctrl Pts',(-2.28396628040981E-16,34.2419663837872,
10.24));
#22576=CARTESIAN_POINT('Ctrl Pts',(3.73,32.7351420011818,11.1000672611831));
#22577=CARTESIAN_POINT('Ctrl Pts',(3.73,33.045415593,10.5747121186603));
#22578=CARTESIAN_POINT('Ctrl Pts',(3.73,33.63686551036,10.24));
#22579=CARTESIAN_POINT('Ctrl Pts',(3.73,34.2419663837872,10.24));
#22580=CARTESIAN_POINT('Ctrl Pts',(3.73,32.7351420011818,14.8300672611831));
#22581=CARTESIAN_POINT('Ctrl Pts',(3.73,33.045415593,14.3047121186603));
#22582=CARTESIAN_POINT('Ctrl Pts',(3.73,33.63686551036,13.97));
#22583=CARTESIAN_POINT('Ctrl Pts',(3.73,34.2419663837872,13.97));
#22584=CARTESIAN_POINT('Ctrl Pts',(0.,32.7351420011818,14.8300672611831));
#22585=CARTESIAN_POINT('Ctrl Pts',(0.,33.045415593,14.3047121186603));
#22586=CARTESIAN_POINT('Ctrl Pts',(0.,33.63686551036,13.97));
#22587=CARTESIAN_POINT('Ctrl Pts',(0.,34.2419663837872,13.97));
#22588=CARTESIAN_POINT('Origin',(0.,34.2419663837872,12.105));
#22589=CARTESIAN_POINT('Origin',(0.,34.2419663837872,12.105));
#22590=CARTESIAN_POINT('Origin',(0.,71.2419663837872,12.105));
#22591=CARTESIAN_POINT('Ctrl Pts',(0.,71.2419663837872,13.97));
#22592=CARTESIAN_POINT('Ctrl Pts',(0.,71.847073728999,13.97));
#22593=CARTESIAN_POINT('Ctrl Pts',(0.,72.4385298261441,14.3047192784616));
#22594=CARTESIAN_POINT('Ctrl Pts',(0.,72.7488007217793,14.8300841178694));
#22595=CARTESIAN_POINT('Ctrl Pts',(-3.73,71.2419663837872,13.97));
#22596=CARTESIAN_POINT('Ctrl Pts',(-3.73,71.847073728999,13.97));
#22597=CARTESIAN_POINT('Ctrl Pts',(-3.73,72.4385298261441,14.3047192784616));
#22598=CARTESIAN_POINT('Ctrl Pts',(-3.73,72.7488007217793,14.8300841178694));
#22599=CARTESIAN_POINT('Ctrl Pts',(-3.73,71.2419663837872,10.24));
#22600=CARTESIAN_POINT('Ctrl Pts',(-3.73,71.847073728999,10.24));
#22601=CARTESIAN_POINT('Ctrl Pts',(-3.73,72.4385298261441,10.5747192784616));
#22602=CARTESIAN_POINT('Ctrl Pts',(-3.73,72.7488007217793,11.1000841178694));
#22603=CARTESIAN_POINT('Ctrl Pts',(-2.28396628040981E-16,71.2419663837872,
10.24));
#22604=CARTESIAN_POINT('Ctrl Pts',(-2.28396628040981E-16,71.847073728999,
10.24));
#22605=CARTESIAN_POINT('Ctrl Pts',(-2.28396628040981E-16,72.4385298261441,
10.5747192784616));
#22606=CARTESIAN_POINT('Ctrl Pts',(-2.28396628040981E-16,72.7488007217793,
11.1000841178694));
#22607=CARTESIAN_POINT('Ctrl Pts',(3.73,71.2419663837872,10.24));
#22608=CARTESIAN_POINT('Ctrl Pts',(3.73,71.847073728999,10.24));
#22609=CARTESIAN_POINT('Ctrl Pts',(3.73,72.4385298261441,10.5747192784616));
#22610=CARTESIAN_POINT('Ctrl Pts',(3.73,72.7488007217793,11.1000841178694));
#22611=CARTESIAN_POINT('Ctrl Pts',(3.73,71.2419663837872,13.97));
#22612=CARTESIAN_POINT('Ctrl Pts',(3.73,71.847073728999,13.97));
#22613=CARTESIAN_POINT('Ctrl Pts',(3.73,72.4385298261441,14.3047192784616));
#22614=CARTESIAN_POINT('Ctrl Pts',(3.73,72.7488007217793,14.8300841178694));
#22615=CARTESIAN_POINT('Ctrl Pts',(0.,71.2419663837872,13.97));
#22616=CARTESIAN_POINT('Ctrl Pts',(0.,71.847073728999,13.97));
#22617=CARTESIAN_POINT('Ctrl Pts',(0.,72.4385298261441,14.3047192784616));
#22618=CARTESIAN_POINT('Ctrl Pts',(0.,72.7488007217793,14.8300841178694));
#22619=CARTESIAN_POINT('Ctrl Pts',(-8.71689482662896,32.7351420011818,11.9977764420206));
#22620=CARTESIAN_POINT('Ctrl Pts',(-8.40809882163708,33.045415593,11.5727552036367));
#22621=CARTESIAN_POINT('Ctrl Pts',(-8.21135997452595,33.63686551036,11.3019674114179));
#22622=CARTESIAN_POINT('Ctrl Pts',(-8.21135997452595,34.2419663837872,11.3019674114179));
#22623=CARTESIAN_POINT('Ctrl Pts',(-11.7345282156475,32.7351420011818,9.80533745096963));
#22624=CARTESIAN_POINT('Ctrl Pts',(-11.4257322106552,33.045415593,9.38031621258576));
#22625=CARTESIAN_POINT('Ctrl Pts',(-11.2289933635445,33.63686551036,9.10952842036699));
#22626=CARTESIAN_POINT('Ctrl Pts',(-11.2289933635445,34.2419663837872,9.10952842036699));
#22627=CARTESIAN_POINT('Ctrl Pts',(-9.54208922459654,32.7351420011818,6.7877040619511));
#22628=CARTESIAN_POINT('Ctrl Pts',(-9.23329321960506,33.045415593,6.36268282356722));
#22629=CARTESIAN_POINT('Ctrl Pts',(-9.03655437249353,33.63686551036,6.09189503134845));
#22630=CARTESIAN_POINT('Ctrl Pts',(-9.03655437249353,34.2419663837872,6.09189503134846));
#22631=CARTESIAN_POINT('Ctrl Pts',(-6.52445583557801,32.7351420011818,8.98014305300205));
#22632=CARTESIAN_POINT('Ctrl Pts',(-6.21565983058692,33.045415593,8.55512181461817));
#22633=CARTESIAN_POINT('Ctrl Pts',(-6.018920983475,33.63686551036,8.28433402239941));
#22634=CARTESIAN_POINT('Ctrl Pts',(-6.018920983475,34.2419663837872,8.28433402239941));
#22635=CARTESIAN_POINT('Ctrl Pts',(-3.50682244655947,32.7351420011818,11.172582044053));
#22636=CARTESIAN_POINT('Ctrl Pts',(-3.19802644156878,33.045415593,10.7475608056691));
#22637=CARTESIAN_POINT('Ctrl Pts',(-3.00128759445646,33.63686551036,10.4767730134504));
#22638=CARTESIAN_POINT('Ctrl Pts',(-3.00128759445646,34.2419663837872,10.4767730134504));
#22639=CARTESIAN_POINT('Ctrl Pts',(-5.69926143761042,32.7351420011818,14.1902154330715));
#22640=CARTESIAN_POINT('Ctrl Pts',(-5.39046543261894,33.045415593,13.7651941946877));
#22641=CARTESIAN_POINT('Ctrl Pts',(-5.19372658550741,33.63686551036,13.4944064024689));
#22642=CARTESIAN_POINT('Ctrl Pts',(-5.19372658550741,34.2419663837872,13.4944064024689));
#22643=CARTESIAN_POINT('Ctrl Pts',(-8.71689482662896,32.7351420011818,11.9977764420206));
#22644=CARTESIAN_POINT('Ctrl Pts',(-8.40809882163708,33.045415593,11.5727552036367));
#22645=CARTESIAN_POINT('Ctrl Pts',(-8.21135997452595,33.63686551036,11.3019674114179));
#22646=CARTESIAN_POINT('Ctrl Pts',(-8.21135997452595,34.2419663837872,11.3019674114179));
#22647=CARTESIAN_POINT('Origin',(-7.11514047900047,34.2419663837872,9.79315071690868));
#22648=CARTESIAN_POINT('Origin',(-7.11514047900047,34.2419663837872,9.79315071690868));
#22649=CARTESIAN_POINT('Origin',(-7.11514047900048,71.2419663837872,9.79315071690868));
#22650=CARTESIAN_POINT('Ctrl Pts',(-8.21135997452595,71.2419663837872,11.3019674114179));
#22651=CARTESIAN_POINT('Ctrl Pts',(-8.21135997452595,71.847073728999,11.3019674114179));
#22652=CARTESIAN_POINT('Ctrl Pts',(-8.40810303006371,72.4385298261441,11.5727609960379));
#22653=CARTESIAN_POINT('Ctrl Pts',(-8.71690473474057,72.7488007217793,11.9977900793663));
#22654=CARTESIAN_POINT('Ctrl Pts',(-11.2289933635445,71.2419663837872,9.10952842036699));
#22655=CARTESIAN_POINT('Ctrl Pts',(-11.2289933635445,71.847073728999,9.10952842036699));
#22656=CARTESIAN_POINT('Ctrl Pts',(-11.4257364190824,72.4385298261441,9.38032200498695));
#22657=CARTESIAN_POINT('Ctrl Pts',(-11.7345381237591,72.7488007217793,9.80535108831532));
#22658=CARTESIAN_POINT('Ctrl Pts',(-9.03655437249354,71.2419663837872,6.09189503134846));
#22659=CARTESIAN_POINT('Ctrl Pts',(-9.03655437249354,71.847073728999,6.09189503134846));
#22660=CARTESIAN_POINT('Ctrl Pts',(-9.23329742803116,72.4385298261441,6.36268861596841));
#22661=CARTESIAN_POINT('Ctrl Pts',(-9.54209913270815,72.7488007217793,6.78771769929678));
#22662=CARTESIAN_POINT('Ctrl Pts',(-6.018920983475,71.2419663837872,8.28433402239941));
#22663=CARTESIAN_POINT('Ctrl Pts',(-6.018920983475,71.847073728999,8.28433402239941));
#22664=CARTESIAN_POINT('Ctrl Pts',(-6.2156640390125,72.4385298261441,8.55512760701937));
#22665=CARTESIAN_POINT('Ctrl Pts',(-6.52446574368962,72.7488007217793,8.98015669034773));
#22666=CARTESIAN_POINT('Ctrl Pts',(-3.00128759445646,71.2419663837872,10.4767730134504));
#22667=CARTESIAN_POINT('Ctrl Pts',(-3.00128759445646,71.847073728999,10.4767730134504));
#22668=CARTESIAN_POINT('Ctrl Pts',(-3.19803064999383,72.4385298261441,10.7475665980703));
#22669=CARTESIAN_POINT('Ctrl Pts',(-3.50683235467108,72.7488007217793,11.1725956813987));
#22670=CARTESIAN_POINT('Ctrl Pts',(-5.19372658550742,71.2419663837872,13.4944064024689));
#22671=CARTESIAN_POINT('Ctrl Pts',(-5.19372658550742,71.847073728999,13.4944064024689));
#22672=CARTESIAN_POINT('Ctrl Pts',(-5.39046964104504,72.4385298261441,13.7651999870889));
#22673=CARTESIAN_POINT('Ctrl Pts',(-5.69927134572203,72.7488007217793,14.1902290704172));
#22674=CARTESIAN_POINT('Ctrl Pts',(-8.21135997452595,71.2419663837872,11.3019674114179));
#22675=CARTESIAN_POINT('Ctrl Pts',(-8.21135997452595,71.847073728999,11.3019674114179));
#22676=CARTESIAN_POINT('Ctrl Pts',(-8.40810303006371,72.4385298261441,11.5727609960379));
#22677=CARTESIAN_POINT('Ctrl Pts',(-8.71690473474057,72.7488007217793,11.9977900793663));
#22678=CARTESIAN_POINT('Ctrl Pts',(-14.1042321058437,32.7351420011818,4.58274281142898));
#22679=CARTESIAN_POINT('Ctrl Pts',(-13.6045896741761,33.045415593,4.42039914430651));
#22680=CARTESIAN_POINT('Ctrl Pts',(-13.2862595326433,33.63686551036,4.31696741141789));
#22681=CARTESIAN_POINT('Ctrl Pts',(-13.2862595326433,34.2419663837872,4.31696741141789));
#22682=CARTESIAN_POINT('Ctrl Pts',(-15.2568654948622,32.7351420011818,1.03530200564804));
#22683=CARTESIAN_POINT('Ctrl Pts',(-14.7572230631946,33.045415593,0.872958338525508));
#22684=CARTESIAN_POINT('Ctrl Pts',(-14.4388929216619,33.63686551036,0.769526605636954));
#22685=CARTESIAN_POINT('Ctrl Pts',(-14.4388929216619,34.2419663837872,0.769526605636955));
#22686=CARTESIAN_POINT('Ctrl Pts',(-11.7094246890812,32.7351420011818,-0.117331383370479));
#22687=CARTESIAN_POINT('Ctrl Pts',(-11.2097822574136,33.045415593,-0.27967505049288));
#22688=CARTESIAN_POINT('Ctrl Pts',(-10.8914521158809,33.63686551036,-0.383106783381566));
#22689=CARTESIAN_POINT('Ctrl Pts',(-10.8914521158809,34.2419663837872,-0.383106783381565));
#22690=CARTESIAN_POINT('Ctrl Pts',(-10.5567913000627,32.7351420011818,3.43010942241045));
#22691=CARTESIAN_POINT('Ctrl Pts',(-10.0571488683951,33.045415593,3.26776575528812));
#22692=CARTESIAN_POINT('Ctrl Pts',(-9.7388187268624,33.63686551036,3.16433402239937));
#22693=CARTESIAN_POINT('Ctrl Pts',(-9.7388187268624,34.2419663837872,3.16433402239937));
#22694=CARTESIAN_POINT('Ctrl Pts',(-9.4041579110442,32.7351420011818,6.97755022819139));
#22695=CARTESIAN_POINT('Ctrl Pts',(-8.9045154793766,33.045415593,6.81520656106912));
#22696=CARTESIAN_POINT('Ctrl Pts',(-8.58618533784388,33.63686551036,6.7117748281803));
#22697=CARTESIAN_POINT('Ctrl Pts',(-8.58618533784388,34.2419663837872,6.7117748281803));
#22698=CARTESIAN_POINT('Ctrl Pts',(-12.9515987168251,32.7351420011818,8.13018361720991));
#22699=CARTESIAN_POINT('Ctrl Pts',(-12.4519562851575,33.045415593,7.96783995008751));
#22700=CARTESIAN_POINT('Ctrl Pts',(-12.1336261436248,33.63686551036,7.86440821719883));
#22701=CARTESIAN_POINT('Ctrl Pts',(-12.1336261436248,34.2419663837872,7.86440821719883));
#22702=CARTESIAN_POINT('Ctrl Pts',(-14.1042321058437,32.7351420011818,4.58274281142898));
#22703=CARTESIAN_POINT('Ctrl Pts',(-13.6045896741761,33.045415593,4.42039914430651));
#22704=CARTESIAN_POINT('Ctrl Pts',(-13.2862595326433,33.63686551036,4.31696741141789));
#22705=CARTESIAN_POINT('Ctrl Pts',(-13.2862595326433,34.2419663837872,4.31696741141789));
#22706=CARTESIAN_POINT('Origin',(-11.5125391297529,34.2419663837872,3.74065071690863));
#22707=CARTESIAN_POINT('Origin',(-11.5125391297529,34.2419663837872,3.74065071690863));
#22708=CARTESIAN_POINT('Origin',(-11.5125391297529,71.2419663837872,3.74065071690863));
#22709=CARTESIAN_POINT('Ctrl Pts',(-13.2862595326433,71.2419663837872,4.31696741141789));
#22710=CARTESIAN_POINT('Ctrl Pts',(-13.2862595326433,71.847073728999,4.31696741141789));
#22711=CARTESIAN_POINT('Ctrl Pts',(-13.6045964835519,72.4385298261441,4.42040135680733));
#22712=CARTESIAN_POINT('Ctrl Pts',(-14.104248137505,72.7488007217793,4.58274802043151));
#22713=CARTESIAN_POINT('Ctrl Pts',(-14.4388929216619,71.2419663837872,0.769526605636955));
#22714=CARTESIAN_POINT('Ctrl Pts',(-14.4388929216619,71.847073728999,0.769526605636955));
#22715=CARTESIAN_POINT('Ctrl Pts',(-14.7572298725705,72.4385298261441,0.872960551026527));
#22716=CARTESIAN_POINT('Ctrl Pts',(-15.2568815265235,72.7488007217793,1.03530721465058));
#22717=CARTESIAN_POINT('Ctrl Pts',(-10.8914521158809,71.2419663837872,-0.383106783381565));
#22718=CARTESIAN_POINT('Ctrl Pts',(-10.8914521158809,71.847073728999,-0.383106783381565));
#22719=CARTESIAN_POINT('Ctrl Pts',(-11.2097890667895,72.4385298261441,-0.279672837992126));
#22720=CARTESIAN_POINT('Ctrl Pts',(-11.7094407207426,72.7488007217793,-0.117326174367942));
#22721=CARTESIAN_POINT('Ctrl Pts',(-9.7388187268624,71.2419663837872,3.16433402239937));
#22722=CARTESIAN_POINT('Ctrl Pts',(-9.7388187268624,71.847073728999,3.16433402239937));
#22723=CARTESIAN_POINT('Ctrl Pts',(-10.057155677771,72.4385298261441,3.26776796778881));
#22724=CARTESIAN_POINT('Ctrl Pts',(-10.5568073317241,72.7488007217793,3.43011463141299));
#22725=CARTESIAN_POINT('Ctrl Pts',(-8.58618533784388,71.2419663837872,6.7117748281803));
#22726=CARTESIAN_POINT('Ctrl Pts',(-8.58618533784388,71.847073728999,6.7117748281803));
#22727=CARTESIAN_POINT('Ctrl Pts',(-8.90452228875249,72.4385298261441,6.81520877356975));
#22728=CARTESIAN_POINT('Ctrl Pts',(-9.40417394270555,72.7488007217793,6.97755543719393));
#22729=CARTESIAN_POINT('Ctrl Pts',(-12.1336261436248,71.2419663837872,7.86440821719883));
#22730=CARTESIAN_POINT('Ctrl Pts',(-12.1336261436248,71.847073728999,7.86440821719883));
#22731=CARTESIAN_POINT('Ctrl Pts',(-12.4519630945334,72.4385298261441,7.96784216258813));
#22732=CARTESIAN_POINT('Ctrl Pts',(-12.9516147484865,72.7488007217793,8.13018882621245));
#22733=CARTESIAN_POINT('Ctrl Pts',(-13.2862595326433,71.2419663837872,4.31696741141789));
#22734=CARTESIAN_POINT('Ctrl Pts',(-13.2862595326433,71.847073728999,4.31696741141789));
#22735=CARTESIAN_POINT('Ctrl Pts',(-13.6045964835519,72.4385298261441,4.42040135680733));
#22736=CARTESIAN_POINT('Ctrl Pts',(-14.104248137505,72.7488007217793,4.58274802043151));
#22737=CARTESIAN_POINT('Ctrl Pts',(-14.1042321058436,32.7351420011818,-4.58274281142927));
#22738=CARTESIAN_POINT('Ctrl Pts',(-13.604589674176,33.045415593,-4.42039914430733));
#22739=CARTESIAN_POINT('Ctrl Pts',(-13.2862595326432,33.63686551036,-4.31696741141817));
#22740=CARTESIAN_POINT('Ctrl Pts',(-13.2862595326432,34.2419663837872,-4.31696741141817));
#22741=CARTESIAN_POINT('Ctrl Pts',(-12.951598716825,32.7351420011818,-8.13018361721019));
#22742=CARTESIAN_POINT('Ctrl Pts',(-12.4519562851574,33.045415593,-7.96783995008897));
#22743=CARTESIAN_POINT('Ctrl Pts',(-12.1336261436246,33.63686551036,-7.86440821719908));
#22744=CARTESIAN_POINT('Ctrl Pts',(-12.1336261436247,34.2419663837872,-7.86440821719908));
#22745=CARTESIAN_POINT('Ctrl Pts',(-9.40415791104406,32.7351420011818,-6.97755022819159));
#22746=CARTESIAN_POINT('Ctrl Pts',(-8.90451547937646,33.045415593,-6.81520656107025));
#22747=CARTESIAN_POINT('Ctrl Pts',(-8.58618533784374,33.63686551036,-6.71177482818048));
#22748=CARTESIAN_POINT('Ctrl Pts',(-8.58618533784374,34.2419663837872,-6.71177482818048));
#22749=CARTESIAN_POINT('Ctrl Pts',(-10.5567913000627,32.7351420011818,-3.43010942241068));
#22750=CARTESIAN_POINT('Ctrl Pts',(-10.0571488683951,33.045415593,-3.26776575528914));
#22751=CARTESIAN_POINT('Ctrl Pts',(-9.73881872686233,33.63686551036,-3.16433402239957));
#22752=CARTESIAN_POINT('Ctrl Pts',(-9.73881872686234,34.2419663837872,-3.16433402239957));
#22753=CARTESIAN_POINT('Ctrl Pts',(-11.7094246890813,32.7351420011818,0.117331383370231));
#22754=CARTESIAN_POINT('Ctrl Pts',(-11.2097822574137,33.045415593,0.279675050491972));
#22755=CARTESIAN_POINT('Ctrl Pts',(-10.8914521158809,33.63686551036,0.383106783381337));
#22756=CARTESIAN_POINT('Ctrl Pts',(-10.8914521158809,34.2419663837872,0.383106783381337));
#22757=CARTESIAN_POINT('Ctrl Pts',(-15.2568654948622,32.7351420011818,-1.03530200564836));
#22758=CARTESIAN_POINT('Ctrl Pts',(-14.7572230631946,33.045415593,-0.872958338525696));
#22759=CARTESIAN_POINT('Ctrl Pts',(-14.4388929216618,33.63686551036,-0.769526605637257));
#22760=CARTESIAN_POINT('Ctrl Pts',(-14.4388929216618,34.2419663837872,-0.769526605637258));
#22761=CARTESIAN_POINT('Ctrl Pts',(-14.1042321058436,32.7351420011818,-4.58274281142927));
#22762=CARTESIAN_POINT('Ctrl Pts',(-13.604589674176,33.045415593,-4.42039914430733));
#22763=CARTESIAN_POINT('Ctrl Pts',(-13.2862595326432,33.63686551036,-4.31696741141817));
#22764=CARTESIAN_POINT('Ctrl Pts',(-13.2862595326432,34.2419663837872,-4.31696741141817));
#22765=CARTESIAN_POINT('Origin',(-11.5125391297528,34.2419663837872,-3.74065071690887));
#22766=CARTESIAN_POINT('Origin',(-11.5125391297528,34.2419663837872,-3.74065071690887));
#22767=CARTESIAN_POINT('Origin',(-11.5125391297528,71.2419663837872,-3.74065071690887));
#22768=CARTESIAN_POINT('Ctrl Pts',(-13.2862595326432,71.2419663837872,-4.31696741141817));
#22769=CARTESIAN_POINT('Ctrl Pts',(-13.2862595326432,71.847073728999,-4.31696741141817));
#22770=CARTESIAN_POINT('Ctrl Pts',(-13.6045964835518,72.4385298261441,-4.42040135680736));
#22771=CARTESIAN_POINT('Ctrl Pts',(-14.1042481375049,72.7488007217793,-4.5827480204318));
#22772=CARTESIAN_POINT('Ctrl Pts',(-12.1336261436247,71.2419663837872,-7.86440821719908));
#22773=CARTESIAN_POINT('Ctrl Pts',(-12.1336261436247,71.847073728999,-7.86440821719908));
#22774=CARTESIAN_POINT('Ctrl Pts',(-12.4519630945332,72.4385298261441,-7.96784216258827));
#22775=CARTESIAN_POINT('Ctrl Pts',(-12.9516147484863,72.7488007217793,-8.13018882621271));
#22776=CARTESIAN_POINT('Ctrl Pts',(-8.58618533784374,71.2419663837872,-6.71177482818048));
#22777=CARTESIAN_POINT('Ctrl Pts',(-8.58618533784374,71.847073728999,-6.71177482818048));
#22778=CARTESIAN_POINT('Ctrl Pts',(-8.90452228875233,72.4385298261441,-6.81520877356967));
#22779=CARTESIAN_POINT('Ctrl Pts',(-9.40417394270539,72.7488007217793,-6.97755543719412));
#22780=CARTESIAN_POINT('Ctrl Pts',(-9.73881872686234,71.2419663837872,-3.16433402239957));
#22781=CARTESIAN_POINT('Ctrl Pts',(-9.73881872686234,71.847073728999,-3.16433402239957));
#22782=CARTESIAN_POINT('Ctrl Pts',(-10.0571556777709,72.4385298261441,-3.26776796778876));
#22783=CARTESIAN_POINT('Ctrl Pts',(-10.556807331724,72.7488007217793,-3.43011463141321));
#22784=CARTESIAN_POINT('Ctrl Pts',(-10.8914521158809,71.2419663837872,0.383106783381337));
#22785=CARTESIAN_POINT('Ctrl Pts',(-10.8914521158809,71.847073728999,0.383106783381337));
#22786=CARTESIAN_POINT('Ctrl Pts',(-11.2097890667895,72.4385298261441,0.279672837992146));
#22787=CARTESIAN_POINT('Ctrl Pts',(-11.7094407207426,72.7488007217793,0.117326174367701));
#22788=CARTESIAN_POINT('Ctrl Pts',(-14.4388929216618,71.2419663837872,-0.769526605637258));
#22789=CARTESIAN_POINT('Ctrl Pts',(-14.4388929216618,71.847073728999,-0.769526605637258));
#22790=CARTESIAN_POINT('Ctrl Pts',(-14.7572298725704,72.4385298261441,-0.872960551026448));
#22791=CARTESIAN_POINT('Ctrl Pts',(-15.2568815265235,72.7488007217793,-1.03530721465089));
#22792=CARTESIAN_POINT('Ctrl Pts',(-13.2862595326432,71.2419663837872,-4.31696741141817));
#22793=CARTESIAN_POINT('Ctrl Pts',(-13.2862595326432,71.847073728999,-4.31696741141817));
#22794=CARTESIAN_POINT('Ctrl Pts',(-13.6045964835518,72.4385298261441,-4.42040135680736));
#22795=CARTESIAN_POINT('Ctrl Pts',(-14.1042481375049,72.7488007217793,-4.5827480204318));
#22796=CARTESIAN_POINT('Ctrl Pts',(-8.71689482662869,32.7351420011818,-11.9977764420208));
#22797=CARTESIAN_POINT('Ctrl Pts',(-8.40809882163841,33.045415593,-11.5727552036369));
#22798=CARTESIAN_POINT('Ctrl Pts',(-8.2113599745257,33.63686551036,-11.3019674114181));
#22799=CARTESIAN_POINT('Ctrl Pts',(-8.2113599745257,34.2419663837872,-11.3019674114181));
#22800=CARTESIAN_POINT('Ctrl Pts',(-5.69926143761011,32.7351420011818,-14.1902154330717));
#22801=CARTESIAN_POINT('Ctrl Pts',(-5.39046543262022,33.045415593,-13.7651941946878));
#22802=CARTESIAN_POINT('Ctrl Pts',(-5.19372658550712,33.63686551036,-13.494406402469));
#22803=CARTESIAN_POINT('Ctrl Pts',(-5.19372658550712,34.2419663837872,-13.494406402469));
#22804=CARTESIAN_POINT('Ctrl Pts',(-3.50682244655923,32.7351420011818,-11.1725820440531));
#22805=CARTESIAN_POINT('Ctrl Pts',(-3.19802644156854,33.045415593,-10.7475608056692));
#22806=CARTESIAN_POINT('Ctrl Pts',(-3.00128759445623,33.63686551036,-10.4767730134504));
#22807=CARTESIAN_POINT('Ctrl Pts',(-3.00128759445624,34.2419663837872,-10.4767730134504));
#22808=CARTESIAN_POINT('Ctrl Pts',(-6.52445583557781,32.7351420011818,-8.98014305300219));
#22809=CARTESIAN_POINT('Ctrl Pts',(-6.21565983058673,33.045415593,-8.55512181461832));
#22810=CARTESIAN_POINT('Ctrl Pts',(-6.01892098347482,33.63686551036,-8.28433402239954));
#22811=CARTESIAN_POINT('Ctrl Pts',(-6.01892098347482,34.2419663837872,-8.28433402239954));
#22812=CARTESIAN_POINT('Ctrl Pts',(-9.54208922459639,32.7351420011818,-6.78770406195131));
#22813=CARTESIAN_POINT('Ctrl Pts',(-9.23329321960491,33.045415593,-6.36268282356744));
#22814=CARTESIAN_POINT('Ctrl Pts',(-9.0365543724934,33.63686551036,-6.09189503134865));
#22815=CARTESIAN_POINT('Ctrl Pts',(-9.0365543724934,34.2419663837872,-6.09189503134866));
#22816=CARTESIAN_POINT('Ctrl Pts',(-11.7345282156473,32.7351420011818,-9.80533745096989));
#22817=CARTESIAN_POINT('Ctrl Pts',(-11.4257322106566,33.045415593,-9.38031621258602));
#22818=CARTESIAN_POINT('Ctrl Pts',(-11.2289933635443,33.63686551036,-9.10952842036724));
#22819=CARTESIAN_POINT('Ctrl Pts',(-11.2289933635443,34.2419663837872,-9.10952842036724));
#22820=CARTESIAN_POINT('Ctrl Pts',(-8.71689482662869,32.7351420011818,-11.9977764420208));
#22821=CARTESIAN_POINT('Ctrl Pts',(-8.40809882163841,33.045415593,-11.5727552036369));
#22822=CARTESIAN_POINT('Ctrl Pts',(-8.2113599745257,33.63686551036,-11.3019674114181));
#22823=CARTESIAN_POINT('Ctrl Pts',(-8.2113599745257,34.2419663837872,-11.3019674114181));
#22824=CARTESIAN_POINT('Origin',(-7.11514047900026,34.2419663837872,-9.79315071690883));
#22825=CARTESIAN_POINT('Origin',(-7.11514047900026,34.2419663837872,-9.79315071690883));
#22826=CARTESIAN_POINT('Origin',(-7.11514047900026,71.2419663837872,-9.79315071690883));
#22827=CARTESIAN_POINT('Ctrl Pts',(-8.2113599745257,71.2419663837872,-11.3019674114181));
#22828=CARTESIAN_POINT('Ctrl Pts',(-8.2113599745257,71.847073728999,-11.3019674114181));
#22829=CARTESIAN_POINT('Ctrl Pts',(-8.40810303006345,72.4385298261441,-11.5727609960386));
#22830=CARTESIAN_POINT('Ctrl Pts',(-8.71690473474031,72.7488007217793,-11.9977900793665));
#22831=CARTESIAN_POINT('Ctrl Pts',(-5.19372658550712,71.2419663837872,-13.494406402469));
#22832=CARTESIAN_POINT('Ctrl Pts',(-5.19372658550712,71.847073728999,-13.494406402469));
#22833=CARTESIAN_POINT('Ctrl Pts',(-5.390469641045,72.4385298261441,-13.7651999870895));
#22834=CARTESIAN_POINT('Ctrl Pts',(-5.69927134572172,72.7488007217793,-14.1902290704173));
#22835=CARTESIAN_POINT('Ctrl Pts',(-3.00128759445624,71.2419663837872,-10.4767730134504));
#22836=CARTESIAN_POINT('Ctrl Pts',(-3.00128759445624,71.847073728999,-10.4767730134504));
#22837=CARTESIAN_POINT('Ctrl Pts',(-3.19803064999385,72.4385298261441,-10.7475665980709));
#22838=CARTESIAN_POINT('Ctrl Pts',(-3.50683235467084,72.7488007217793,-11.1725956813988));
#22839=CARTESIAN_POINT('Ctrl Pts',(-6.01892098347482,71.2419663837872,-8.28433402239954));
#22840=CARTESIAN_POINT('Ctrl Pts',(-6.01892098347482,71.847073728999,-8.28433402239954));
#22841=CARTESIAN_POINT('Ctrl Pts',(-6.2156640390123,72.4385298261441,-8.55512760702004));
#22842=CARTESIAN_POINT('Ctrl Pts',(-6.52446574368942,72.7488007217793,-8.98015669034787));
#22843=CARTESIAN_POINT('Ctrl Pts',(-9.0365543724934,71.2419663837872,-6.09189503134866));
#22844=CARTESIAN_POINT('Ctrl Pts',(-9.0365543724934,71.847073728999,-6.09189503134866));
#22845=CARTESIAN_POINT('Ctrl Pts',(-9.23329742803075,72.4385298261441,-6.36268861596915));
#22846=CARTESIAN_POINT('Ctrl Pts',(-9.542099132708,72.7488007217793,-6.78771769929699));
#22847=CARTESIAN_POINT('Ctrl Pts',(-11.2289933635443,71.2419663837872,-9.10952842036724));
#22848=CARTESIAN_POINT('Ctrl Pts',(-11.2289933635443,71.847073728999,-9.10952842036724));
#22849=CARTESIAN_POINT('Ctrl Pts',(-11.4257364190819,72.4385298261441,-9.38032200498773));
#22850=CARTESIAN_POINT('Ctrl Pts',(-11.7345381237589,72.7488007217793,-9.80535108831557));
#22851=CARTESIAN_POINT('Ctrl Pts',(-8.2113599745257,71.2419663837872,-11.3019674114181));
#22852=CARTESIAN_POINT('Ctrl Pts',(-8.2113599745257,71.847073728999,-11.3019674114181));
#22853=CARTESIAN_POINT('Ctrl Pts',(-8.40810303006345,72.4385298261441,-11.5727609960386));
#22854=CARTESIAN_POINT('Ctrl Pts',(-8.71690473474031,72.7488007217793,-11.9977900793665));
#22855=CARTESIAN_POINT('Ctrl Pts',(2.4156304102994,5.,10.8339636164256));
#22856=CARTESIAN_POINT('Ctrl Pts',(2.41563040646342,4.96191046202733,10.8339636166853));
#22857=CARTESIAN_POINT('Ctrl Pts',(2.4146547402783,4.92371376427368,10.8341812987099));
#22858=CARTESIAN_POINT('Ctrl Pts',(2.41072929832241,4.84720274160474,10.8350554324849));
#22859=CARTESIAN_POINT('Ctrl Pts',(2.40775787877141,4.80871695881661,10.8357166882541));
#22860=CARTESIAN_POINT('Ctrl Pts',(2.39988157827119,4.73242631317627,10.8374638426754));
#22861=CARTESIAN_POINT('Ctrl Pts',(2.39497737791963,4.6945034108209,10.8385495849069));
#22862=CARTESIAN_POINT('Ctrl Pts',(2.38327169996162,4.61914358580643,10.8411295401524));
#22863=CARTESIAN_POINT('Ctrl Pts',(2.37647039420389,4.58169825793974,10.8426237055241));
#22864=CARTESIAN_POINT('Ctrl Pts',(2.35325442553652,4.47005693394489,10.847694801622));
#22865=CARTESIAN_POINT('Ctrl Pts',(2.3340338175079,4.39655416040346,10.8518604682163));
#22866=CARTESIAN_POINT('Ctrl Pts',(2.29959460874979,4.28768080804602,10.8591914690199));
#22867=CARTESIAN_POINT('Ctrl Pts',(2.28717862543041,4.25162018871417,10.8618155803769));
#22868=CARTESIAN_POINT('Ctrl Pts',(2.26045417586942,4.17996386393482,10.8674086381803));
#22869=CARTESIAN_POINT('Ctrl Pts',(2.24614896131211,4.14437664773035,10.8703769337531));
#22870=CARTESIAN_POINT('Ctrl Pts',(2.22323683546441,4.09132438210188,10.8750777516754));
#22871=CARTESIAN_POINT('Ctrl Pts',(2.21535159730481,4.07368696613903,10.876687111824));
#22872=CARTESIAN_POINT('Ctrl Pts',(2.19918231004094,4.03871821508943,10.8799679279219));
#22873=CARTESIAN_POINT('Ctrl Pts',(2.19088543945954,4.0213559005185,10.881642029533));
#22874=CARTESIAN_POINT('Ctrl Pts',(2.1653921502188,3.96969451639992,10.8867540523146));
#22875=CARTESIAN_POINT('Ctrl Pts',(2.14756476939503,3.93575377943081,10.8902875627326));
#22876=CARTESIAN_POINT('Ctrl Pts',(2.09168081411357,3.83552515343858,10.9012085469626));
#22877=CARTESIAN_POINT('Ctrl Pts',(2.05118520112225,3.77072933843846,10.9089252412181));
#22878=CARTESIAN_POINT('Ctrl Pts',(1.9856514830744,3.67657009081119,10.9209760193803));
#22879=CARTESIAN_POINT('Ctrl Pts',(1.96300593858833,3.64568758622464,10.9250725911264));
#22880=CARTESIAN_POINT('Ctrl Pts',(1.91610256695852,3.58493352527622,10.9333962768342));
#22881=CARTESIAN_POINT('Ctrl Pts',(1.8918447870784,3.55506189924222,10.9376234277111));
#22882=CARTESIAN_POINT('Ctrl Pts',(1.84169472079833,3.49634022773492,10.9461793901794));
#22883=CARTESIAN_POINT('Ctrl Pts',(1.81579980814473,3.46748730973486,10.950508647301));
#22884=CARTESIAN_POINT('Ctrl Pts',(1.762350359702,3.41083271569288,10.9592376624932));
#22885=CARTESIAN_POINT('Ctrl Pts',(1.7350155020693,3.38326334323313,10.9636014218412));
#22886=CARTESIAN_POINT('Ctrl Pts',(1.67913447380159,3.3295910796627,10.9722988530446));
#22887=CARTESIAN_POINT('Ctrl Pts',(1.65059069640107,3.30349081702451,10.976632138154));
#22888=CARTESIAN_POINT('Ctrl Pts',(1.59231052652113,3.25274008369802,10.9852378081031));
#22889=CARTESIAN_POINT('Ctrl Pts',(1.56257408110084,3.22808968398168,10.9895102305428));
#22890=CARTESIAN_POINT('Ctrl Pts',(1.47158319578018,3.15629691321311,11.0021919668541));
#22891=CARTESIAN_POINT('Ctrl Pts',(1.4085487056756,3.11130657146225,11.0104663920413));
#22892=CARTESIAN_POINT('Ctrl Pts',(1.31039752202577,3.04816755746305,11.0224307105556));
#22893=CARTESIAN_POINT('Ctrl Pts',(1.27707162401967,3.02784269906396,11.026345142236));
#22894=CARTESIAN_POINT('Ctrl Pts',(1.20921161545083,2.98867493489448,11.0339932853651));
#22895=CARTESIAN_POINT('Ctrl Pts',(1.17462206754654,2.96980348548508,11.0377327364982));
#22896=CARTESIAN_POINT('Ctrl Pts',(1.10437191556843,2.93366312106671,11.0449827080004));
#22897=CARTESIAN_POINT('Ctrl Pts',(1.06896163113932,2.91651856790947,11.0484679583694));
#22898=CARTESIAN_POINT('Ctrl Pts',(0.99745210450957,2.8839794871732,11.0551532019847));
#22899=CARTESIAN_POINT('Ctrl Pts',(0.961374437599674,2.86859606260606,11.0583509995041));
#22900=CARTESIAN_POINT('Ctrl Pts',(0.852182302673737,2.82507151370299,11.0674818389069));
#22901=CARTESIAN_POINT('Ctrl Pts',(0.778110692064935,2.79955051761125,11.072952549289));
#22902=CARTESIAN_POINT('Ctrl Pts',(0.627408873998724,2.75548409895438,11.0825128433466));
#22903=CARTESIAN_POINT('Ctrl Pts',(0.550764519707227,2.73694017621321,11.0866023912725));
#22904=CARTESIAN_POINT('Ctrl Pts',(0.453346626462258,2.71823575173535,11.0907572215327));
#22905=CARTESIAN_POINT('Ctrl Pts',(0.433768364290407,2.71471972381952,11.091540182064));
#22906=CARTESIAN_POINT('Ctrl Pts',(0.394471422995838,2.70814371620271,11.0930073608194));
#22907=CARTESIAN_POINT('Ctrl Pts',(0.374709949322281,2.70507888898263,11.0936926629967));
#22908=CARTESIAN_POINT('Ctrl Pts',(0.315428279537668,2.69661093714137,11.0955891856498));
#22909=CARTESIAN_POINT('Ctrl Pts',(0.275950761088858,2.69193338400005,11.0966410913946));
#22910=CARTESIAN_POINT('Ctrl Pts',(0.196982185499563,2.68446381383399,11.0983237617));
#22911=CARTESIAN_POINT('Ctrl Pts',(0.15750785306126,2.6816738708479,11.0989540709247));
#22912=CARTESIAN_POINT('Ctrl Pts',(0.0785788629130702,2.67796041583801,
11.0997934908188));
#22913=CARTESIAN_POINT('Ctrl Pts',(0.0391242055410394,2.67703693714379,
11.1000026010139));
#22914=CARTESIAN_POINT('Ctrl Pts',(-0.0397655306445661,2.67704700686668,
11.1000003220684));
#22915=CARTESIAN_POINT('Ctrl Pts',(-0.0792006094009493,2.67798056075966,
11.0997889324828));
#22916=CARTESIAN_POINT('Ctrl Pts',(-0.158051149433861,2.68170867442521,
11.0989462083064));
#22917=CARTESIAN_POINT('Ctrl Pts',(-0.197466610929021,2.68450321228798,
11.0983148732779));
#22918=CARTESIAN_POINT('Ctrl Pts',(-0.276277740964502,2.691970802071,11.0966326754737));
#22919=CARTESIAN_POINT('Ctrl Pts',(-0.315692244683293,2.6966476678611,11.0955809556022));
#22920=CARTESIAN_POINT('Ctrl Pts',(-0.394425801998236,2.70789613574509,
11.0930617027531));
#22921=CARTESIAN_POINT('Ctrl Pts',(-0.433929268879025,2.71450588894859,
11.0915857051179));
#22922=CARTESIAN_POINT('Ctrl Pts',(-0.512099892385214,2.72951817727644,
11.088251080714));
#22923=CARTESIAN_POINT('Ctrl Pts',(-0.550844005958438,2.73792358666081,
11.0863917748127));
#22924=CARTESIAN_POINT('Ctrl Pts',(-0.627648551372376,2.75650099223247,
11.0823088358929));
#22925=CARTESIAN_POINT('Ctrl Pts',(-0.665711553652418,2.76667258968464,
11.0800852864604));
#22926=CARTESIAN_POINT('Ctrl Pts',(-0.778896822997667,2.79980374463825,
11.0728980009129));
#22927=CARTESIAN_POINT('Ctrl Pts',(-0.853017446172679,2.82537397001114,
11.0674174899872));
#22928=CARTESIAN_POINT('Ctrl Pts',(-0.962206209010363,2.86894308941064,
11.0582786539946));
#22929=CARTESIAN_POINT('Ctrl Pts',(-0.998269898716162,2.88433653123043,
11.0550793011122));
#22930=CARTESIAN_POINT('Ctrl Pts',(-1.06972690046675,2.91688220503822,11.0483938054367));
#22931=CARTESIAN_POINT('Ctrl Pts',(-1.10511644984475,2.93403302039874,11.0449079354868));
#22932=CARTESIAN_POINT('Ctrl Pts',(-1.15770183492388,2.96110559714924,11.0394778777837));
#22933=CARTESIAN_POINT('Ctrl Pts',(-1.17516443843644,2.97036515149108,11.0376322386051));
#22934=CARTESIAN_POINT('Ctrl Pts',(-1.2097533438837,2.98924572661077,11.0338947272429));
#22935=CARTESIAN_POINT('Ctrl Pts',(-1.22689739274055,2.99887498930594,11.0320011655461));
#22936=CARTESIAN_POINT('Ctrl Pts',(-1.27783270600622,3.02829829309359,11.0262569913433));
#22937=CARTESIAN_POINT('Ctrl Pts',(-1.31119618898078,3.04866234676234,11.0223358849783));
#22938=CARTESIAN_POINT('Ctrl Pts',(-1.40939028702048,3.11188658794701,11.0103586558181));
#22939=CARTESIAN_POINT('Ctrl Pts',(-1.47245317748874,3.15693830849233,11.0020755577165));
#22940=CARTESIAN_POINT('Ctrl Pts',(-1.56344017683738,3.22879604108859,10.9893870450015));
#22941=CARTESIAN_POINT('Ctrl Pts',(-1.59317047816761,3.25346508699623,10.9851130961949));
#22942=CARTESIAN_POINT('Ctrl Pts',(-1.65142959479989,3.30424588822654,10.9765059300651));
#22943=CARTESIAN_POINT('Ctrl Pts',(-1.67995846001316,3.33035757709127,10.9721726752733));
#22944=CARTESIAN_POINT('Ctrl Pts',(-1.73580177581937,3.38404418683126,10.9634769150375));
#22945=CARTESIAN_POINT('Ctrl Pts',(-1.76310394536657,3.41160605178525,10.9591164076345));
#22946=CARTESIAN_POINT('Ctrl Pts',(-1.81652054390736,3.46827741771502,10.950389075345));
#22947=CARTESIAN_POINT('Ctrl Pts',(-1.84243547813984,3.49717550469378,10.9460549961774));
#22948=CARTESIAN_POINT('Ctrl Pts',(-1.91759973418787,3.58528425276366,10.9332254057859));
#22949=CARTESIAN_POINT('Ctrl Pts',(-1.96446790094007,3.64607226263407,10.924873889815));
#22950=CARTESIAN_POINT('Ctrl Pts',(-2.05174009021352,3.77158859432735,10.9088206765596));
#22951=CARTESIAN_POINT('Ctrl Pts',(-2.09216488383321,3.83633288700501,10.901115442483));
#22952=CARTESIAN_POINT('Ctrl Pts',(-2.16654149406423,3.96984994441741,10.8865775716981));
#22953=CARTESIAN_POINT('Ctrl Pts',(-2.20049638474852,4.03862680065782,10.8797440406559));
#22954=CARTESIAN_POINT('Ctrl Pts',(-2.26167466414558,4.18036900107911,10.8671908711269));
#22955=CARTESIAN_POINT('Ctrl Pts',(-2.28842901591865,4.25224727888041,10.861569105968));
#22956=CARTESIAN_POINT('Ctrl Pts',(-2.32294443531106,4.36156646287466,10.8542206101891));
#22957=CARTESIAN_POINT('Ctrl Pts',(-2.33351137927865,4.39825592106845,10.8519518627414));
#22958=CARTESIAN_POINT('Ctrl Pts',(-2.35276891893271,4.47213522058744,10.8477930062897));
#22959=CARTESIAN_POINT('Ctrl Pts',(-2.36145955719913,4.50932505011558,10.8459028807817));
#22960=CARTESIAN_POINT('Ctrl Pts',(-2.37695087388553,4.58420950581499,10.842518395405));
#22961=CARTESIAN_POINT('Ctrl Pts',(-2.38375121930333,4.62190806642754,10.8410241061104));
#22962=CARTESIAN_POINT('Ctrl Pts',(-2.39543543506865,4.69780231164114,10.8384483539548));
#22963=CARTESIAN_POINT('Ctrl Pts',(-2.40032026602255,4.73607758644075,10.8373666666763));
#22964=CARTESIAN_POINT('Ctrl Pts',(-2.4080591253686,4.81229232838475,10.8356497156866));
#22965=CARTESIAN_POINT('Ctrl Pts',(-2.41094073121308,4.85039249837638,10.8350083744313));
#22966=CARTESIAN_POINT('Ctrl Pts',(-2.41474521241477,4.92648239506272,10.8341611253141));
#22967=CARTESIAN_POINT('Ctrl Pts',(-2.41567073860182,4.96448834035588,10.8339546120371));
#22968=CARTESIAN_POINT('Ctrl Pts',(-2.41554570444982,5.07839028587593,10.8339825280547));
#22969=CARTESIAN_POINT('Ctrl Pts',(-2.41159986026808,5.15417063580015,10.8348645066324));
#22970=CARTESIAN_POINT('Ctrl Pts',(-2.39987263492885,5.26760931939004,10.8374657949017));
#22971=CARTESIAN_POINT('Ctrl Pts',(-2.3949939379871,5.30538351494416,10.8385459312144));
#22972=CARTESIAN_POINT('Ctrl Pts',(-2.38327313722814,5.38085361371876,10.8411292271885));
#22973=CARTESIAN_POINT('Ctrl Pts',(-2.37643605907484,5.41852509424237,10.842631312589));
#22974=CARTESIAN_POINT('Ctrl Pts',(-2.36074019728461,5.49388602647724,10.8460595647364));
#22975=CARTESIAN_POINT('Ctrl Pts',(-2.35192727742988,5.53133066944476,10.847975598964));
#22976=CARTESIAN_POINT('Ctrl Pts',(-2.33249514119272,5.60538197638679,10.8521704144231));
#22977=CARTESIAN_POINT('Ctrl Pts',(-2.32185976834581,5.64206644689879,10.8544527161351));
#22978=CARTESIAN_POINT('Ctrl Pts',(-2.28725682906933,5.75104027067158,10.8618161407086));
#22979=CARTESIAN_POINT('Ctrl Pts',(-2.26058751143076,5.82230286023678,10.8674161778334));
#22980=CARTESIAN_POINT('Ctrl Pts',(-2.20012765225572,5.96207070793676,10.879817410451));
#22981=CARTESIAN_POINT('Ctrl Pts',(-2.16632117305358,6.03059585160356,10.8866217931097));
#22982=CARTESIAN_POINT('Ctrl Pts',(-2.11021062948697,6.13124662702467,10.8975875763066));
#22983=CARTESIAN_POINT('Ctrl Pts',(-2.09055922533177,6.16450059218788,10.9013776540111));
#22984=CARTESIAN_POINT('Ctrl Pts',(-2.0495249337574,6.23010608733983,10.9091667943008));
#22985=CARTESIAN_POINT('Ctrl Pts',(-2.02827774511065,6.26224430958768,10.9131400653633));
#22986=CARTESIAN_POINT('Ctrl Pts',(-1.98427798089149,6.32533987135752,10.921226002024));
#22987=CARTESIAN_POINT('Ctrl Pts',(-1.96153794828895,6.35627729755836,10.9253362970998));
#22988=CARTESIAN_POINT('Ctrl Pts',(-1.91459588826076,6.41695053601302,10.9336602605952));
#22989=CARTESIAN_POINT('Ctrl Pts',(-1.89039379550754,6.44668629011437,10.9378739665585));
#22990=CARTESIAN_POINT('Ctrl Pts',(-1.81560525975469,6.53410605383734,10.9506242215266));
#22991=CARTESIAN_POINT('Ctrl Pts',(-1.76282588318345,6.59001917192089,10.9592724352714));
#22992=CARTESIAN_POINT('Ctrl Pts',(-1.67929121916504,6.67026153860375,10.9722747191892));
#22993=CARTESIAN_POINT('Ctrl Pts',(-1.65068440659162,6.69642949301749,10.9766184770752));
#22994=CARTESIAN_POINT('Ctrl Pts',(-1.60668911510993,6.73473798863923,10.9831145720195));
#22995=CARTESIAN_POINT('Ctrl Pts',(-1.5918286735277,6.74736125538106,10.9852786585169));
#22996=CARTESIAN_POINT('Ctrl Pts',(-1.56173096481231,6.77229914034996,10.9895979272402));
#22997=CARTESIAN_POINT('Ctrl Pts',(-1.54649511948918,6.78461114468206,10.9917527484078));
#22998=CARTESIAN_POINT('Ctrl Pts',(-1.50046299609324,6.8208863539386,10.9981636505124));
#22999=CARTESIAN_POINT('Ctrl Pts',(-1.46926889933719,6.8442557123388,11.0023772465835));
#23000=CARTESIAN_POINT('Ctrl Pts',(-1.4058819134907,6.88939440371742,11.0106562928922));
#23001=CARTESIAN_POINT('Ctrl Pts',(-1.37368942458412,6.91116409133562,11.014721793832));
#23002=CARTESIAN_POINT('Ctrl Pts',(-1.27562769998999,6.97410209399274,11.0266560937395));
#23003=CARTESIAN_POINT('Ctrl Pts',(-1.20827745529124,7.01290459305882,11.0342629589178));
#23004=CARTESIAN_POINT('Ctrl Pts',(-1.10427269937667,7.06637670145155,11.0449911598163));
#23005=CARTESIAN_POINT('Ctrl Pts',(-1.06910708126474,7.08341081377451,11.0484536090625));
#23006=CARTESIAN_POINT('Ctrl Pts',(-0.997767307365202,7.1158814910318,11.0551244811633));
#23007=CARTESIAN_POINT('Ctrl Pts',(-0.961574891490949,7.13132421016612,
11.0583342396346));
#23008=CARTESIAN_POINT('Ctrl Pts',(-0.888233537645138,7.16055810015767,
11.0644671680054));
#23009=CARTESIAN_POINT('Ctrl Pts',(-0.850905427704504,7.174408118809,11.0674029783619));
#23010=CARTESIAN_POINT('Ctrl Pts',(-0.775972604593802,7.20017590695015,
11.0729086838722));
#23011=CARTESIAN_POINT('Ctrl Pts',(-0.738304539072183,7.21212774105555,
11.0754854863593));
#23012=CARTESIAN_POINT('Ctrl Pts',(-0.662579844985102,7.23419056906833,
11.0802734702955));
#23013=CARTESIAN_POINT('Ctrl Pts',(-0.624521775547128,7.24430304346141,
11.082484955623));
#23014=CARTESIAN_POINT('Ctrl Pts',(-0.548017474289304,7.26270849228187,
11.0865313321938));
#23015=CARTESIAN_POINT('Ctrl Pts',(-0.509571237699919,7.27100144163261,
11.0883662321975));
#23016=CARTESIAN_POINT('Ctrl Pts',(-0.432291130932363,7.28577276473672,
11.0916478861797));
#23017=CARTESIAN_POINT('Ctrl Pts',(-0.393457261520405,7.29225114048083,
11.0930946487716));
#23018=CARTESIAN_POINT('Ctrl Pts',(-0.315399720419757,7.30338509498235,
11.095588332377));
#23019=CARTESIAN_POINT('Ctrl Pts',(-0.276176055080666,7.30804070294351,
11.0966352622835));
#23020=CARTESIAN_POINT('Ctrl Pts',(-0.197333992891634,7.31550747812966,
11.0983172863715));
#23021=CARTESIAN_POINT('Ctrl Pts',(-0.157704437931099,7.31831807552468,
11.0989522478944));
#23022=CARTESIAN_POINT('Ctrl Pts',(-0.0780874231236657,7.32206150143807,
11.0997984477102));
#23023=CARTESIAN_POINT('Ctrl Pts',(-0.0379603180932254,7.32298838989236,
11.1000083329759));
#23024=CARTESIAN_POINT('Ctrl Pts',(0.0417241354210129,7.32292629716545,
11.099994280309));
#23025=CARTESIAN_POINT('Ctrl Pts',(0.0814525850909876,7.32194969219772,
11.0997731475059));
#23026=CARTESIAN_POINT('Ctrl Pts',(0.160590954427694,7.31813222019943,11.0989102633425));
#23027=CARTESIAN_POINT('Ctrl Pts',(0.20001689949773,7.31529243258597,11.0982687691481));
#23028=CARTESIAN_POINT('Ctrl Pts',(0.317869850089211,7.30401006241601,11.0957274457278));
#23029=CARTESIAN_POINT('Ctrl Pts',(0.39587285156736,7.29281046628245,11.0932107509896));
#23030=CARTESIAN_POINT('Ctrl Pts',(0.512030046125537,7.27049131741402,11.0882532445282));
#23031=CARTESIAN_POINT('Ctrl Pts',(0.550607673542793,7.26213015717154,11.086403628318));
#23032=CARTESIAN_POINT('Ctrl Pts',(0.627477206669618,7.24354385437346,11.0823186508056));
#23033=CARTESIAN_POINT('Ctrl Pts',(0.665755064237897,7.23332253883107,11.0800840952145));
#23034=CARTESIAN_POINT('Ctrl Pts',(0.722996099836931,7.21655528832399,11.0764469056906));
#23035=CARTESIAN_POINT('Ctrl Pts',(0.742042918675023,7.21072650572253,11.0751869081376));
#23036=CARTESIAN_POINT('Ctrl Pts',(0.779849633212899,7.19865927796806,11.0725889483452));
#23037=CARTESIAN_POINT('Ctrl Pts',(0.798649001180196,7.19240958846945,11.0712485432115));
#23038=CARTESIAN_POINT('Ctrl Pts',(0.854666863641607,7.17304031601826,11.067112468226));
#23039=CARTESIAN_POINT('Ctrl Pts',(0.891570912702515,7.15928178548173,11.0641978059314));
#23040=CARTESIAN_POINT('Ctrl Pts',(1.00088099062815,7.11554187341872,11.0550267106888));
#23041=CARTESIAN_POINT('Ctrl Pts',(1.07196896812727,7.0830775621415,11.0483378721597));
#23042=CARTESIAN_POINT('Ctrl Pts',(1.21057840344948,7.01162593460114,11.0340105647525));
#23043=CARTESIAN_POINT('Ctrl Pts',(1.27812692254345,6.97261769660203,11.0263679610096));
#23044=CARTESIAN_POINT('Ctrl Pts',(1.37669697349307,6.90916978481267,11.0143471976774));
#23045=CARTESIAN_POINT('Ctrl Pts',(1.40914141553145,6.88715448579056,11.0102403439491));
#23046=CARTESIAN_POINT('Ctrl Pts',(1.47300711921128,6.8415030610202,11.0018780835753));
#23047=CARTESIAN_POINT('Ctrl Pts',(1.50419107014757,6.81803676660196,10.997653926145));
#23048=CARTESIAN_POINT('Ctrl Pts',(1.56518118183191,6.76978651362157,10.9891396747484));
#23049=CARTESIAN_POINT('Ctrl Pts',(1.59497278844201,6.74501293387364,10.9848514749544));
#23050=CARTESIAN_POINT('Ctrl Pts',(1.65317070166917,6.69418444296186,10.976243756771));
#23051=CARTESIAN_POINT('Ctrl Pts',(1.68157694109886,6.66812947486887,10.9719242010104));
#23052=CARTESIAN_POINT('Ctrl Pts',(1.76473424719298,6.58805129410511,10.9589642510358));
#23053=CARTESIAN_POINT('Ctrl Pts',(1.81743452458119,6.53211093866748,10.9503210215531));
#23054=CARTESIAN_POINT('Ctrl Pts',(1.89232452431014,6.44435373899584,10.9375402227472));
#23055=CARTESIAN_POINT('Ctrl Pts',(1.91660671007598,6.41443993771718,10.933308141626));
#23056=CARTESIAN_POINT('Ctrl Pts',(1.95195872350825,6.36860811698971,10.9270323866911));
#23057=CARTESIAN_POINT('Ctrl Pts',(1.96357402652069,6.35315622680682,10.9249507025615));
#23058=CARTESIAN_POINT('Ctrl Pts',(1.98643628446213,6.3219390979067,10.9208169219368));
#23059=CARTESIAN_POINT('Ctrl Pts',(1.9977042602328,6.30614290086018,10.9187609319534));
#23060=CARTESIAN_POINT('Ctrl Pts',(2.03081608796765,6.25847073177151,10.9126681102492));
#23061=CARTESIAN_POINT('Ctrl Pts',(2.05198092012552,6.22630457810867,10.9087046566163));
#23062=CARTESIAN_POINT('Ctrl Pts',(2.09256316418001,6.16115702982226,10.9009927356767));
#23063=CARTESIAN_POINT('Ctrl Pts',(2.11197419513562,6.12818538630473,10.8972454344251));
#23064=CARTESIAN_POINT('Ctrl Pts',(2.16759831848063,6.02808738494578,10.8863668497116));
#23065=CARTESIAN_POINT('Ctrl Pts',(2.20120809777231,5.95978047562522,10.8795986198096));
#23066=CARTESIAN_POINT('Ctrl Pts',(2.2614896280558,5.82000298645159,10.8672282185851));
#23067=CARTESIAN_POINT('Ctrl Pts',(2.2881589362429,5.74852711829037,10.8616262047409));
#23068=CARTESIAN_POINT('Ctrl Pts',(2.31704068721011,5.65715216261029,10.8554776448299));
#23069=CARTESIAN_POINT('Ctrl Pts',(2.32259192245271,5.63877136657054,10.854291036586));
#23070=CARTESIAN_POINT('Ctrl Pts',(2.33324304840448,5.60180732026267,10.8520064569235));
#23071=CARTESIAN_POINT('Ctrl Pts',(2.33834431821141,5.5832109511349,10.8509081711304));
#23072=CARTESIAN_POINT('Ctrl Pts',(2.35288057231345,5.52742057732017,10.84776883442));
#23073=CARTESIAN_POINT('Ctrl Pts',(2.36157792726873,5.49014214904587,10.8458770896334));
#23074=CARTESIAN_POINT('Ctrl Pts',(2.3770239137965,5.41539753514177,10.8425023671237));
#23075=CARTESIAN_POINT('Ctrl Pts',(2.38377222451045,5.37793487473886,10.8410194554346));
#23076=CARTESIAN_POINT('Ctrl Pts',(2.39534115048824,5.30283063923535,10.8384691587443));
#23077=CARTESIAN_POINT('Ctrl Pts',(2.40016173520365,5.26518906149763,10.8374017701789));
#23078=CARTESIAN_POINT('Ctrl Pts',(2.40788262248997,5.18972752394682,10.8356889400362));
#23079=CARTESIAN_POINT('Ctrl Pts',(2.4107829231545,5.1519075640333,10.8350434949868));
#23080=CARTESIAN_POINT('Ctrl Pts',(2.41465680569752,5.07608856983399,10.8341808348376));
#23081=CARTESIAN_POINT('Ctrl Pts',(2.41563041413539,5.03808953797268,10.8339636161659));
#23082=CARTESIAN_POINT('Ctrl Pts',(2.4156304102994,5.,10.8339636164256));
#23083=CARTESIAN_POINT('Ctrl Pts',(1.99999329969225,5.,10.4183265058185));
#23084=CARTESIAN_POINT('Ctrl Pts',(1.99999329651629,4.9672060898008,10.4183265060683));
#23085=CARTESIAN_POINT('Ctrl Pts',(1.99918550496642,4.93431991835465,10.4185358368808));
#23086=CARTESIAN_POINT('Ctrl Pts',(1.99593548063469,4.8684463021299,10.4193764351511));
#23087=CARTESIAN_POINT('Ctrl Pts',(1.99347532813476,4.83531123743932,10.4200123223252));
#23088=CARTESIAN_POINT('Ctrl Pts',(1.98695423610042,4.76962735899715,10.4216924484417));
#23089=CARTESIAN_POINT('Ctrl Pts',(1.9828938600587,4.73697691689266,10.4227365369645));
#23090=CARTESIAN_POINT('Ctrl Pts',(1.97320227918419,4.67209444612268,10.4252175141091));
#23091=CARTESIAN_POINT('Ctrl Pts',(1.96757121663137,4.63985518083304,10.4266543569164));
#23092=CARTESIAN_POINT('Ctrl Pts',(1.94834982349861,4.5437354653307,10.4315309041118));
#23093=CARTESIAN_POINT('Ctrl Pts',(1.93243634306278,4.48045185824893,10.4355367579463));
#23094=CARTESIAN_POINT('Ctrl Pts',(1.90392279791606,4.38671528043056,10.442586510252));
#23095=CARTESIAN_POINT('Ctrl Pts',(1.89364312792087,4.35566820621918,10.4451099494912));
#23096=CARTESIAN_POINT('Ctrl Pts',(1.87151692855195,4.29397433422457,10.4504884337122));
#23097=CARTESIAN_POINT('Ctrl Pts',(1.8596730913725,4.26333484541557,10.4533428527908));
#23098=CARTESIAN_POINT('Ctrl Pts',(1.84070326139284,4.21765849102848,10.4578633272628));
#23099=CARTESIAN_POINT('Ctrl Pts',(1.83417476952651,4.20247322320904,10.4594109454833));
#23100=CARTESIAN_POINT('Ctrl Pts',(1.82078759487817,4.1723662137063,10.4625658954651));
#23101=CARTESIAN_POINT('Ctrl Pts',(1.8139182967022,4.15741779964833,10.4641757713891));
#23102=CARTESIAN_POINT('Ctrl Pts',(1.79281142230163,4.11293895107949,10.469091675146));
#23103=CARTESIAN_POINT('Ctrl Pts',(1.77805144823985,4.08371702979842,10.4724896250146));
#23104=CARTESIAN_POINT('Ctrl Pts',(1.73178297287775,3.99742329311597,10.4829916336515));
#23105=CARTESIAN_POINT('Ctrl Pts',(1.69825509779176,3.94163610714523,10.4904122825615));
#23106=CARTESIAN_POINT('Ctrl Pts',(1.64399721279419,3.86056791689028,10.5020007414106));
#23107=CARTESIAN_POINT('Ctrl Pts',(1.62524809577395,3.83397903878751,10.5059401511702));
#23108=CARTESIAN_POINT('Ctrl Pts',(1.58641499092785,3.78167167763213,10.5139445047481));
#23109=CARTESIAN_POINT('Ctrl Pts',(1.56633104223321,3.7559531345937,10.5180094840654));
#23110=CARTESIAN_POINT('Ctrl Pts',(1.52480987404805,3.70539559767788,10.5262372032753));
#23111=CARTESIAN_POINT('Ctrl Pts',(1.50337048018112,3.68055413064413,10.5304003716057));
#23112=CARTESIAN_POINT('Ctrl Pts',(1.45911762663949,3.63177628328041,10.538794504498));
#23113=CARTESIAN_POINT('Ctrl Pts',(1.43648604695728,3.60803990912586,10.5429908514021));
#23114=CARTESIAN_POINT('Ctrl Pts',(1.39021999498227,3.56182975575039,10.5513546120022));
#23115=CARTESIAN_POINT('Ctrl Pts',(1.36658750414032,3.53935823956277,10.5555216537896));
#23116=CARTESIAN_POINT('Ctrl Pts',(1.31833511057554,3.4956634330663,10.563797173489));
#23117=CARTESIAN_POINT('Ctrl Pts',(1.29371516402102,3.4744402038623,10.5679056875586));
#23118=CARTESIAN_POINT('Ctrl Pts',(1.21838031138833,3.41262885610495,10.5801008983079));
#23119=CARTESIAN_POINT('Ctrl Pts',(1.16619163330238,3.3738935679989,10.588057881209));
#23120=CARTESIAN_POINT('Ctrl Pts',(1.0849284943634,3.3195328362764,10.5995631973718));
#23121=CARTESIAN_POINT('Ctrl Pts',(1.05733670199568,3.30203376391625,10.6033274547364));
#23122=CARTESIAN_POINT('Ctrl Pts',(1.00115279162757,3.26831153442107,10.6106821824337));
#23123=CARTESIAN_POINT('Ctrl Pts',(0.972514774920624,3.25206380209878,10.6142781722521));
#23124=CARTESIAN_POINT('Ctrl Pts',(0.91435197292097,3.22094806984305,10.6212500038866));
#23125=CARTESIAN_POINT('Ctrl Pts',(0.885034436887127,3.20618714160478,10.6246015451677));
#23126=CARTESIAN_POINT('Ctrl Pts',(0.825828950189364,3.17817200284419,10.6310303142887));
#23127=CARTESIAN_POINT('Ctrl Pts',(0.795958862538632,3.16492735167072,10.6341054306391));
#23128=CARTESIAN_POINT('Ctrl Pts',(0.705554495503631,3.12745406571931,10.6428859720493));
#23129=CARTESIAN_POINT('Ctrl Pts',(0.644227760967397,3.10548128005308,10.6481468026185));
#23130=CARTESIAN_POINT('Ctrl Pts',(0.519455931177073,3.06754146105868,10.6573403229691));
#23131=CARTESIAN_POINT('Ctrl Pts',(0.455999123235534,3.05157571903715,10.6612729783714));
#23132=CARTESIAN_POINT('Ctrl Pts',(0.375343103600641,3.03547178999415,10.6652684116006));
#23133=CARTESIAN_POINT('Ctrl Pts',(0.359133507551698,3.03244459906876,10.6660213344221));
#23134=CARTESIAN_POINT('Ctrl Pts',(0.326598058853661,3.02678286057751,10.6674322259349));
#23135=CARTESIAN_POINT('Ctrl Pts',(0.31023677495422,3.02414413944877,10.6680912369941));
#23136=CARTESIAN_POINT('Ctrl Pts',(0.261155201109811,3.01685349569121,10.6699150009392));
#23137=CARTESIAN_POINT('Ctrl Pts',(0.22847024564255,3.01282626759034,10.6709265510874));
#23138=CARTESIAN_POINT('Ctrl Pts',(0.163089125504509,3.00639519947324,10.6725446669741));
#23139=CARTESIAN_POINT('Ctrl Pts',(0.130406807857837,3.00399314513972,10.6731507948452));
#23140=CARTESIAN_POINT('Ctrl Pts',(0.0650584620285826,3.00079597561227,
10.6739580110074));
#23141=CARTESIAN_POINT('Ctrl Pts',(0.0323924341257924,3.00000088911391,
10.6741590988424));
#23142=CARTESIAN_POINT('Ctrl Pts',(-0.032923411838495,3.00000955883287,
10.6741569073271));
#23143=CARTESIAN_POINT('Ctrl Pts',(-0.0655732298525685,3.00081331976463,
10.6739536275487));
#23144=CARTESIAN_POINT('Ctrl Pts',(-0.130856623814915,3.0040231099398,10.6731432338706));
#23145=CARTESIAN_POINT('Ctrl Pts',(-0.163490199944121,3.0064291203195,10.6725361195498));
#23146=CARTESIAN_POINT('Ctrl Pts',(-0.228740964854252,3.01285848338826,
10.6709184580371));
#23147=CARTESIAN_POINT('Ctrl Pts',(-0.261373748002534,3.0168851197008,10.6699070866313));
#23148=CARTESIAN_POINT('Ctrl Pts',(-0.326560287476677,3.02656970148655,
10.6674844830799));
#23149=CARTESIAN_POINT('Ctrl Pts',(-0.359266726646795,3.03226049388052,
10.6660651110172));
#23150=CARTESIAN_POINT('Ctrl Pts',(-0.423987191574684,3.04518560826949,
10.6628584170459));
#23151=CARTESIAN_POINT('Ctrl Pts',(-0.456064932944746,3.05242240491246,
10.6610704420591));
#23152=CARTESIAN_POINT('Ctrl Pts',(-0.519654369291847,3.06841697461527,
10.6571441421124));
#23153=CARTESIAN_POINT('Ctrl Pts',(-0.551168192433233,3.07717440437623,
10.6550058975318));
#23154=CARTESIAN_POINT('Ctrl Pts',(-0.644878628993597,3.10569930066508,
10.6480943469511));
#23155=CARTESIAN_POINT('Ctrl Pts',(-0.706245942918383,3.12771447121482,
10.6428240918291));
#23156=CARTESIAN_POINT('Ctrl Pts',(-0.796647518071845,3.16522613098054,
10.6340358606123));
#23157=CARTESIAN_POINT('Ctrl Pts',(-0.826506033457877,3.17847940669766,
10.6309592485692));
#23158=CARTESIAN_POINT('Ctrl Pts',(-0.885668032788551,3.20650022188821,
10.6245302370582));
#23159=CARTESIAN_POINT('Ctrl Pts',(-0.914968401476247,3.22126654168918,
10.6211780999659));
#23160=CARTESIAN_POINT('Ctrl Pts',(-0.958505863735288,3.24457519015467,
10.6159563624653));
#23161=CARTESIAN_POINT('Ctrl Pts',(-0.972963824634976,3.25254737910032,
10.6141815298874));
#23162=CARTESIAN_POINT('Ctrl Pts',(-1.00160130942706,3.26880296837598,10.6105874054219));
#23163=CARTESIAN_POINT('Ctrl Pts',(-1.01579552667855,3.27709346474105,10.6087664888383));
#23164=CARTESIAN_POINT('Ctrl Pts',(-1.05796683103677,3.3024260162378,10.6032426856883));
#23165=CARTESIAN_POINT('Ctrl Pts',(-1.08558974144489,3.31995883450879,10.5994720097086));
#23166=CARTESIAN_POINT('Ctrl Pts',(-1.16688841085728,3.37439294419322,10.5879542782074));
#23167=CARTESIAN_POINT('Ctrl Pts',(-1.21910060269637,3.4131810775366,10.579988955122));
#23168=CARTESIAN_POINT('Ctrl Pts',(-1.2944322379834,3.47504835541167,10.5677872279407));
#23169=CARTESIAN_POINT('Ctrl Pts',(-1.31904709760952,3.49628763840776,10.5636772460622));
#23170=CARTESIAN_POINT('Ctrl Pts',(-1.36728206038105,3.54000833243635,10.555400287582));
#23171=CARTESIAN_POINT('Ctrl Pts',(-1.39090220484978,3.5624896862504,10.5512332749491));
#23172=CARTESIAN_POINT('Ctrl Pts',(-1.43713703322785,3.60871219123269,10.542871121211));
#23173=CARTESIAN_POINT('Ctrl Pts',(-1.45974154918718,3.63244210165777,10.5386779014935));
#23174=CARTESIAN_POINT('Ctrl Pts',(-1.5039672050319,3.68123438909642,10.5302853869406));
#23175=CARTESIAN_POINT('Ctrl Pts',(-1.52542317553505,3.70611474522063,10.5261175815582));
#23176=CARTESIAN_POINT('Ctrl Pts',(-1.5876545532419,3.781973643112,10.5137801890434));
#23177=CARTESIAN_POINT('Ctrl Pts',(-1.62645851061903,3.83431023323932,10.5057490728896));
#23178=CARTESIAN_POINT('Ctrl Pts',(-1.69871451180625,3.94237589980096,10.4903117294499));
#23179=CARTESIAN_POINT('Ctrl Pts',(-1.73218375281194,3.99811872665182,10.4829021010573));
#23180=CARTESIAN_POINT('Ctrl Pts',(-1.79376300826393,4.11307276977823,10.4689219650798));
#23181=CARTESIAN_POINT('Ctrl Pts',(-1.8218755678564,4.1722875087188,10.4623505974706));
#23182=CARTESIAN_POINT('Ctrl Pts',(-1.87252741772401,4.29432314473221,10.450279021133));
#23183=CARTESIAN_POINT('Ctrl Pts',(-1.89467837428495,4.3562081113934,10.4448729308931));
#23184=CARTESIAN_POINT('Ctrl Pts',(-1.92325501714616,4.45032853641604,10.4378063547941));
#23185=CARTESIAN_POINT('Ctrl Pts',(-1.93200379636489,4.48191702137343,10.435624646187));
#23186=CARTESIAN_POINT('Ctrl Pts',(-1.94794785391295,4.54552480563549,10.4316253412292));
#23187=CARTESIAN_POINT('Ctrl Pts',(-1.95514316749603,4.57754409478369,10.4298077290074));
#23188=CARTESIAN_POINT('Ctrl Pts',(-1.96796902423475,4.64201728732508,10.4265530869432));
#23189=CARTESIAN_POINT('Ctrl Pts',(-1.97359929168517,4.67447457815043,10.4251161249672));
#23190=CARTESIAN_POINT('Ctrl Pts',(-1.983273103185,4.73981716812693,10.4226391896641));
#23191=CARTESIAN_POINT('Ctrl Pts',(-1.98731744255768,4.77277099197138,10.4215990005289));
#23192=CARTESIAN_POINT('Ctrl Pts',(-1.99372474177576,4.83838951968663,10.4199479191114));
#23193=CARTESIAN_POINT('Ctrl Pts',(-1.99611053405461,4.87119258372489,10.4193311824455));
#23194=CARTESIAN_POINT('Ctrl Pts',(-1.99926041032697,4.93670362354867,10.4185164374226));
#23195=CARTESIAN_POINT('Ctrl Pts',(-2.00002668904448,4.96942556304549,10.4183178468768));
#23196=CARTESIAN_POINT('Ctrl Pts',(-1.99992316846238,5.06749160352923,10.4183446919168));
#23197=CARTESIAN_POINT('Ctrl Pts',(-1.99665625234319,5.13273613319904,10.4191928340298));
#23198=CARTESIAN_POINT('Ctrl Pts',(-1.98694683156342,5.23040331953685,10.4216943257723));
#23199=CARTESIAN_POINT('Ctrl Pts',(-1.98290757077532,5.2629257297,10.4227330234433));
#23200=CARTESIAN_POINT('Ctrl Pts',(-1.9732034691524,5.32790314275541,10.4252172131519));
#23201=CARTESIAN_POINT('Ctrl Pts',(-1.96754278925792,5.36033711846412,10.4266616721418));
#23202=CARTESIAN_POINT('Ctrl Pts',(-1.9545475817628,5.4252205425165,10.4299584018965));
#23203=CARTESIAN_POINT('Ctrl Pts',(-1.94725102655095,5.4574592181287,10.4318009288688));
#23204=CARTESIAN_POINT('Ctrl Pts',(-1.93116241377835,5.52121509544425,10.4358348132929));
#23205=CARTESIAN_POINT('Ctrl Pts',(-1.92235697965934,5.55279928616215,10.4380295561648));
#23206=CARTESIAN_POINT('Ctrl Pts',(-1.8937078757207,5.64662236675201,10.4451104883262));
#23207=CARTESIAN_POINT('Ctrl Pts',(-1.87162732218956,5.70797724494732,10.4504956841121));
#23208=CARTESIAN_POINT('Ctrl Pts',(-1.82157028004747,5.82831302453619,10.462421152487));
#23209=CARTESIAN_POINT('Ctrl Pts',(-1.79358059602456,5.88731104676773,10.4689644899698));
#23210=CARTESIAN_POINT('Ctrl Pts',(-1.74712451951398,5.97396824099842,10.4795095788929));
#23211=CARTESIAN_POINT('Ctrl Pts',(-1.73085436639918,6.00259887306966,10.4831542530315));
#23212=CARTESIAN_POINT('Ctrl Pts',(-1.69688049860201,6.05908316852454,10.4906445686363));
#23213=CARTESIAN_POINT('Ctrl Pts',(-1.67928913414922,6.08675318056602,10.4944654080531));
#23214=CARTESIAN_POINT('Ctrl Pts',(-1.64286003752453,6.14107650126717,10.5022411336526));
#23215=CARTESIAN_POINT('Ctrl Pts',(-1.62403269015965,6.16771266517537,10.5061937402564));
#23216=CARTESIAN_POINT('Ctrl Pts',(-1.58516755370093,6.2199504406717,10.5141983609647));
#23217=CARTESIAN_POINT('Ctrl Pts',(-1.56512971051978,6.2455520021926,10.5182504111727));
#23218=CARTESIAN_POINT('Ctrl Pts',(-1.50320940608863,6.32081770594603,10.5305115119104));
#23219=CARTESIAN_POINT('Ctrl Pts',(-1.45951133081404,6.36895716551933,10.5388279432439));
#23220=CARTESIAN_POINT('Ctrl Pts',(-1.39034977049567,6.43804335315058,10.5513314040246));
#23221=CARTESIAN_POINT('Ctrl Pts',(-1.36666509041035,6.46057314985643,10.5555085168081));
#23222=CARTESIAN_POINT('Ctrl Pts',(-1.33023969693693,6.49355557579673,10.5617553938089));
#23223=CARTESIAN_POINT('Ctrl Pts',(-1.31793616595463,6.50442381673603,10.5638364567065));
#23224=CARTESIAN_POINT('Ctrl Pts',(-1.29301711562714,6.5258945618213,10.5679900198363));
#23225=CARTESIAN_POINT('Ctrl Pts',(-1.28040277345317,6.53649481548491,10.5700621728617));
#23226=CARTESIAN_POINT('Ctrl Pts',(-1.24229100852006,6.56772664496179,10.5762271253839));
#23227=CARTESIAN_POINT('Ctrl Pts',(-1.21646421637671,6.58784693734603,10.5802790699156));
#23228=CARTESIAN_POINT('Ctrl Pts',(-1.16398369351188,6.62670994987825,10.5882404966524));
#23229=CARTESIAN_POINT('Ctrl Pts',(-1.13733029411824,6.64545297536011,10.5921500276145));
#23230=CARTESIAN_POINT('Ctrl Pts',(-1.05614122177108,6.69964064255493,10.6036264768123));
#23231=CARTESIAN_POINT('Ctrl Pts',(-1.00037936451277,6.73304839013043,10.6109415101573));
#23232=CARTESIAN_POINT('Ctrl Pts',(-0.914269828020596,6.77908621610956,
10.6212581314547));
#23233=CARTESIAN_POINT('Ctrl Pts',(-0.885154860638645,6.79375205821659,
10.6245877463615));
#23234=CARTESIAN_POINT('Ctrl Pts',(-0.826089918753355,6.82170830370448,
10.6310026953207));
#23235=CARTESIAN_POINT('Ctrl Pts',(-0.796124826023135,6.83500400566012,
10.6340893137497));
#23236=CARTESIAN_POINT('Ctrl Pts',(-0.7354026991366,6.86017347775672,10.6399869567978));
#23237=CARTESIAN_POINT('Ctrl Pts',(-0.704497321620944,6.87209791402106,
10.6428101369315));
#23238=CARTESIAN_POINT('Ctrl Pts',(-0.642457556136971,6.89428317998444,
10.6481046200665));
#23239=CARTESIAN_POINT('Ctrl Pts',(-0.611270716323594,6.90457333825948,
10.650582565406));
#23240=CARTESIAN_POINT('Ctrl Pts',(-0.548575330411194,6.92356874852439,
10.6551868618314));
#23241=CARTESIAN_POINT('Ctrl Pts',(-0.51706559135898,6.93227527516635,10.6573135051376));
#23242=CARTESIAN_POINT('Ctrl Pts',(-0.453724738693371,6.94812179544253,
10.6612046454231));
#23243=CARTESIAN_POINT('Ctrl Pts',(-0.421893621131155,6.95526176748658,
10.6629691508268));
#23244=CARTESIAN_POINT('Ctrl Pts',(-0.357910449253673,6.96797941829523,
10.666124906548));
#23245=CARTESIAN_POINT('Ctrl Pts',(-0.325758395572844,6.97355709877383,
10.6675161651485));
#23246=CARTESIAN_POINT('Ctrl Pts',(-0.261131555917996,6.98314308809049,
10.6699141804015));
#23247=CARTESIAN_POINT('Ctrl Pts',(-0.228656775201119,6.98715142207219,
10.6709209456059));
#23248=CARTESIAN_POINT('Ctrl Pts',(-0.163380400371696,6.99358008379832,
10.6725384400668));
#23249=CARTESIAN_POINT('Ctrl Pts',(-0.130569568031515,6.99599992093688,
10.6731490417541));
#23250=CARTESIAN_POINT('Ctrl Pts',(-0.0646515801295788,6.99922289448238,
10.6739627777313));
#23251=CARTESIAN_POINT('Ctrl Pts',(-0.0314288069565178,7.00002091667821,
10.6741646109019));
#23252=CARTESIAN_POINT('Ctrl Pts',(0.034545016044109,6.99996745676729,10.6741510973553));
#23253=CARTESIAN_POINT('Ctrl Pts',(0.0674377271166929,6.99912663019606,
10.6739384481509));
#23254=CARTESIAN_POINT('Ctrl Pts',(0.132959426026927,6.99583990526937,10.6731086679089));
#23255=CARTESIAN_POINT('Ctrl Pts',(0.165601681910348,6.99339493625858,10.6724917841714));
#23256=CARTESIAN_POINT('Ctrl Pts',(0.263176671250974,6.98368116565678,10.6700479567701));
#23257=CARTESIAN_POINT('Ctrl Pts',(0.327758355453141,6.97403866093226,10.6676278131896));
#23258=CARTESIAN_POINT('Ctrl Pts',(0.423929363170454,6.95482256636443,10.662860497847));
#23259=CARTESIAN_POINT('Ctrl Pts',(0.455869264250656,6.94762386685945,10.6610818408133));
#23260=CARTESIAN_POINT('Ctrl Pts',(0.51951250642408,6.93162163692076,10.6571535804832));
#23261=CARTESIAN_POINT('Ctrl Pts',(0.551204216520391,6.92282140142685,10.6550047519871));
#23262=CARTESIAN_POINT('Ctrl Pts',(0.598596270858466,6.90838531906186,10.651507100586));
#23263=CARTESIAN_POINT('Ctrl Pts',(0.614365864540558,6.90336691812094,10.6502954419199));
#23264=CARTESIAN_POINT('Ctrl Pts',(0.645667497206255,6.89297740949471,10.6477971509597));
#23265=CARTESIAN_POINT('Ctrl Pts',(0.661232216797669,6.88759662077693,10.6465081694911));
#23266=CARTESIAN_POINT('Ctrl Pts',(0.707611559063241,6.870920278264,10.6425307720051));
#23267=CARTESIAN_POINT('Ctrl Pts',(0.738165840271985,6.85907461042715,10.6397279286031));
#23268=CARTESIAN_POINT('Ctrl Pts',(0.828667856850741,6.82141590347851,10.6309086757391));
#23269=CARTESIAN_POINT('Ctrl Pts',(0.887524326813267,6.79346513890245,10.6244764496207));
#23270=CARTESIAN_POINT('Ctrl Pts',(1.00228440796659,6.73194750487758,10.61069879891));
#23271=CARTESIAN_POINT('Ctrl Pts',(1.05821042421503,6.69836262246893,10.6033493980851));
#23272=CARTESIAN_POINT('Ctrl Pts',(1.13982035950534,6.64373593932943,10.5917898025677));
#23273=CARTESIAN_POINT('Ctrl Pts',(1.166682360582,6.62478145005242,10.587840505287));
#23274=CARTESIAN_POINT('Ctrl Pts',(1.21955923234813,6.58547698998104,10.5797990569321));
#23275=CARTESIAN_POINT('Ctrl Pts',(1.24537762437723,6.5652732386934,10.57573695622));
#23276=CARTESIAN_POINT('Ctrl Pts',(1.29587368296139,6.52373126818002,10.567549347867));
#23277=CARTESIAN_POINT('Ctrl Pts',(1.32053929958603,6.50240198479123,10.5634256617298));
#23278=CARTESIAN_POINT('Ctrl Pts',(1.36872358970513,6.45864023142691,10.555148172375));
#23279=CARTESIAN_POINT('Ctrl Pts',(1.39224220757259,6.43620771243708,10.55099433322));
#23280=CARTESIAN_POINT('Ctrl Pts',(1.4610913387557,6.36726288378714,10.5385315822717));
#23281=CARTESIAN_POINT('Ctrl Pts',(1.50472392477513,6.31909997369742,10.5302199439827));
#23282=CARTESIAN_POINT('Ctrl Pts',(1.56672823513365,6.24354374806328,10.5179294711992));
#23283=CARTESIAN_POINT('Ctrl Pts',(1.58683239039956,6.21778889344791,10.5138597507829));
#23284=CARTESIAN_POINT('Ctrl Pts',(1.6161016816345,6.17832911805555,10.5078247606078));
#23285=CARTESIAN_POINT('Ctrl Pts',(1.62571843761662,6.1650255201114,10.5058229387712));
#23286=CARTESIAN_POINT('Ctrl Pts',(1.64464698003922,6.13814854085892,10.5018477476246));
#23287=CARTESIAN_POINT('Ctrl Pts',(1.65397617044284,6.12454850538974,10.499870634197));
#23288=CARTESIAN_POINT('Ctrl Pts',(1.68139072580193,6.08350424716808,10.4940115591526));
#23289=CARTESIAN_POINT('Ctrl Pts',(1.69891390415089,6.05581018704498,10.4902001605269));
#23290=CARTESIAN_POINT('Ctrl Pts',(1.73251350442475,5.99972016963036,10.4827841018083));
#23291=CARTESIAN_POINT('Ctrl Pts',(1.74858464332341,5.97133260773809,10.4791805630355));
#23292=CARTESIAN_POINT('Ctrl Pts',(1.79463799383422,5.88515133481207,10.4687193272885));
#23293=CARTESIAN_POINT('Ctrl Pts',(1.82246482243469,5.82634120558652,10.4622107555889));
#23294=CARTESIAN_POINT('Ctrl Pts',(1.87237421923056,5.70599712498802,10.4503149357833));
#23295=CARTESIAN_POINT('Ctrl Pts',(1.89445476493774,5.64445862053575,10.444927839113));
#23296=CARTESIAN_POINT('Ctrl Pts',(1.91836707708914,5.56578761925045,10.4390151642179));
#23297=CARTESIAN_POINT('Ctrl Pts',(1.92296315819647,5.54996232425224,10.4378740793336));
#23298=CARTESIAN_POINT('Ctrl Pts',(1.93178163491661,5.5181374274502,10.4356771459032));
#23299=CARTESIAN_POINT('Ctrl Pts',(1.93600517233787,5.50212653071398,10.4346209950434));
#23300=CARTESIAN_POINT('Ctrl Pts',(1.94804029604001,5.45409275014757,10.4316020966957));
#23301=CARTESIAN_POINT('Ctrl Pts',(1.95524117062808,5.42199718022814,10.4297829273177));
#23302=CARTESIAN_POINT('Ctrl Pts',(1.96802949678548,5.35764438713302,10.4265376735752));
#23303=CARTESIAN_POINT('Ctrl Pts',(1.97361668270375,5.32539019906802,10.4251116527113));
#23304=CARTESIAN_POINT('Ctrl Pts',(1.98319504135561,5.26072778293563,10.422659196293));
#23305=CARTESIAN_POINT('Ctrl Pts',(1.98718618879701,5.22831955259754,10.4216327573112));
#23306=CARTESIAN_POINT('Ctrl Pts',(1.99357860825591,5.16334951049017,10.4199856386474));
#23307=CARTESIAN_POINT('Ctrl Pts',(1.99597987869506,5.13078769863434,10.4193649556265));
#23308=CARTESIAN_POINT('Ctrl Pts',(1.99918721500645,5.06550989744515,10.4185353908046));
#23309=CARTESIAN_POINT('Ctrl Pts',(1.99999330286821,5.0327939101992,10.4183265055687));
#23310=CARTESIAN_POINT('Ctrl Pts',(1.99999329969225,5.,10.4183265058185));
#23311=CARTESIAN_POINT('Ctrl Pts',(2.,5.,10.4183332061262));
#23312=CARTESIAN_POINT('Ctrl Pts',(2.41562897926683,5.,10.833962185393));
#23313=CARTESIAN_POINT('Ctrl Pts',(3.59141650529373E-16,7.32295927629177,
-11.1000030851297));
#23314=CARTESIAN_POINT('Ctrl Pts',(-0.0395691838876551,7.32295990573061,
-11.1000032408218));
#23315=CARTESIAN_POINT('Ctrl Pts',(-0.0792480196814607,7.32202355274369,
-11.0997912002962));
#23316=CARTESIAN_POINT('Ctrl Pts',(-0.138851565118895,7.31919772571126,
-11.0991524396978));
#23317=CARTESIAN_POINT('Ctrl Pts',(-0.158753838675174,7.31801677199209,
-11.0988856072371));
#23318=CARTESIAN_POINT('Ctrl Pts',(-0.198581505665056,7.31517650523761,
-11.098244514889));
#23319=CARTESIAN_POINT('Ctrl Pts',(-0.218536420251613,7.31351371080974,
-11.0978694722481));
#23320=CARTESIAN_POINT('Ctrl Pts',(-0.278146117405925,7.30782774736753,
-11.0965886887918));
#23321=CARTESIAN_POINT('Ctrl Pts',(-0.317613541660884,7.30310818992191,
-11.0955274847949));
#23322=CARTESIAN_POINT('Ctrl Pts',(-0.39605519666046,7.29184182175108,-11.0930045053607));
#23323=CARTESIAN_POINT('Ctrl Pts',(-0.435022618201916,7.2852960959019,-11.0915429826038));
#23324=CARTESIAN_POINT('Ctrl Pts',(-0.551175423835523,7.26295715587163,
-11.0865811830642));
#23325=CARTESIAN_POINT('Ctrl Pts',(-0.627612884303839,7.24446796609068,
-11.0825036025914));
#23326=CARTESIAN_POINT('Ctrl Pts',(-0.740782815607558,7.21136052569271,
-11.0753211833526));
#23327=CARTESIAN_POINT('Ctrl Pts',(-0.778258017825594,7.19942761690082,
-11.0727493127705));
#23328=CARTESIAN_POINT('Ctrl Pts',(-0.852708576998866,7.17375101290638,
-11.0672648489048));
#23329=CARTESIAN_POINT('Ctrl Pts',(-0.889689399732524,7.16000413758078,
-11.0643515901889));
#23330=CARTESIAN_POINT('Ctrl Pts',(-0.963122271949541,7.13068279406864,
-11.0582018229929));
#23331=CARTESIAN_POINT('Ctrl Pts',(-0.999664283304993,7.11505987960465,
-11.0549556139893));
#23332=CARTESIAN_POINT('Ctrl Pts',(-1.07137816592919,7.08233580403699,-11.0482356814349));
#23333=CARTESIAN_POINT('Ctrl Pts',(-1.10671472204407,7.06517237057916,-11.0447487888929));
#23334=CARTESIAN_POINT('Ctrl Pts',(-1.17627149074728,7.02930781471142,-11.0375576578648));
#23335=CARTESIAN_POINT('Ctrl Pts',(-1.21050801027134,7.01060045520381,-11.0338520882294));
#23336=CARTESIAN_POINT('Ctrl Pts',(-1.27791136778758,6.97165130432156,-11.0262488851133));
#23337=CARTESIAN_POINT('Ctrl Pts',(-1.31107818901857,6.95140949202481,-11.022351230684));
#23338=CARTESIAN_POINT('Ctrl Pts',(-1.37634819184388,6.90939549569852,-11.0143914369154));
#23339=CARTESIAN_POINT('Ctrl Pts',(-1.40845137292374,6.88762331447492,-11.0103292771151));
#23340=CARTESIAN_POINT('Ctrl Pts',(-1.47159235053576,6.8425412193416,-11.0020680975225));
#23341=CARTESIAN_POINT('Ctrl Pts',(-1.50263016283063,6.81923133219222,-10.9978690567128));
#23342=CARTESIAN_POINT('Ctrl Pts',(-1.56363073599172,6.77105478122795,-10.9893621530921));
#23343=CARTESIAN_POINT('Ctrl Pts',(-1.59358047784877,6.74619913511913,-10.9850561672757));
#23344=CARTESIAN_POINT('Ctrl Pts',(-1.63772444238942,6.70769161663002,-10.9785315012905));
#23345=CARTESIAN_POINT('Ctrl Pts',(-1.65229673063601,6.69466048408886,-10.9763473205741));
#23346=CARTESIAN_POINT('Ctrl Pts',(-1.68100866985036,6.66834339584427,-10.9719867982326));
#23347=CARTESIAN_POINT('Ctrl Pts',(-1.69517895867899,6.65503220446354,-10.9698060775071));
#23348=CARTESIAN_POINT('Ctrl Pts',(-1.76501302384678,6.58778811663768,-10.9589227410546));
#23349=CARTESIAN_POINT('Ctrl Pts',(-1.81781525541685,6.53168602021943,-10.9502589641262));
#23350=CARTESIAN_POINT('Ctrl Pts',(-1.91736851011095,6.41498992816885,-10.9332668766608));
#23351=CARTESIAN_POINT('Ctrl Pts',(-1.96413203779847,6.35438957031199,-10.9249365463836));
#23352=CARTESIAN_POINT('Ctrl Pts',(-2.02973646447202,6.26007175633004,-10.9128704248536));
#23353=CARTESIAN_POINT('Ctrl Pts',(-2.05084657504034,6.2280620392678,-10.9089199119683));
#23354=CARTESIAN_POINT('Ctrl Pts',(-2.09152952892892,6.16288203805261,-10.9011930500009));
#23355=CARTESIAN_POINT('Ctrl Pts',(-2.11109336159131,6.1297281320993,-10.8974184538125));
#23356=CARTESIAN_POINT('Ctrl Pts',(-2.14868711090803,6.06216595808922,-10.8900683089525));
#23357=CARTESIAN_POINT('Ctrl Pts',(-2.16656540913263,6.02802490454898,-10.8865224179582));
#23358=CARTESIAN_POINT('Ctrl Pts',(-2.20043854820833,5.95918844731336,-10.8797263939069));
#23359=CARTESIAN_POINT('Ctrl Pts',(-2.21644946563092,5.92446397243587,-10.8764730840726));
#23360=CARTESIAN_POINT('Ctrl Pts',(-2.26173355722098,5.81939986438648,-10.867179507195));
#23361=CARTESIAN_POINT('Ctrl Pts',(-2.28827057824315,5.74815944124914,-10.861604149854));
#23362=CARTESIAN_POINT('Ctrl Pts',(-2.32262249161282,5.63950759674824,-10.8542913504755));
#23363=CARTESIAN_POINT('Ctrl Pts',(-2.33316279507002,5.6029910482451,-10.8520287182818));
#23364=CARTESIAN_POINT('Ctrl Pts',(-2.35240682804735,5.52935307013381,-10.8478734427179));
#23365=CARTESIAN_POINT('Ctrl Pts',(-2.3611106540472,5.4922316722176,-10.845980778159));
#23366=CARTESIAN_POINT('Ctrl Pts',(-2.37665232084687,5.41737336076027,-10.8425857820485));
#23367=CARTESIAN_POINT('Ctrl Pts',(-2.38349027560913,5.37963617118941,-10.8410834320379));
#23368=CARTESIAN_POINT('Ctrl Pts',(-2.39525550971482,5.30353201909676,-10.8384900627892));
#23369=CARTESIAN_POINT('Ctrl Pts',(-2.40013100120209,5.2655000511311,-10.837410515403));
#23370=CARTESIAN_POINT('Ctrl Pts',(-2.40791064220601,5.18947403914131,-10.8356846557461));
#23371=CARTESIAN_POINT('Ctrl Pts',(-2.41081468487305,5.1514802455297,-10.8350383575405));
#23372=CARTESIAN_POINT('Ctrl Pts',(-2.41467844117742,5.07553057246289,-10.8341779448215));
#23373=CARTESIAN_POINT('Ctrl Pts',(-2.41563806455839,5.03757469469925,-10.8339638311628));
#23374=CARTESIAN_POINT('Ctrl Pts',(-2.41561975408118,4.92376356609547,-10.833967947073));
#23375=CARTESIAN_POINT('Ctrl Pts',(-2.41174928755245,4.84795567679569,-10.8348331281171));
#23376=CARTESIAN_POINT('Ctrl Pts',(-2.40011491936355,4.7343846268852,-10.8374140583306));
#23377=CARTESIAN_POINT('Ctrl Pts',(-2.39525947699857,4.69653011768703,-10.8384891654576));
#23378=CARTESIAN_POINT('Ctrl Pts',(-2.38649876037944,4.63980636344301,-10.8404202936167));
#23379=CARTESIAN_POINT('Ctrl Pts',(-2.38332866809805,4.62089145846394,-10.8411178467378));
#23380=CARTESIAN_POINT('Ctrl Pts',(-2.37649388864143,4.58309623805945,-10.8426181569366));
#23381=CARTESIAN_POINT('Ctrl Pts',(-2.37282073446204,4.56417679276885,-10.843422759711));
#23382=CARTESIAN_POINT('Ctrl Pts',(-2.36109679154098,4.50769073244946,-10.8459838310384));
#23383=CARTESIAN_POINT('Ctrl Pts',(-2.35235033340462,4.47040395413937,-10.8478857353273));
#23384=CARTESIAN_POINT('Ctrl Pts',(-2.33301633666041,4.39647560359754,-10.8520602474027));
#23385=CARTESIAN_POINT('Ctrl Pts',(-2.32243189431414,4.35984750172526,-10.8543321744628));
#23386=CARTESIAN_POINT('Ctrl Pts',(-2.28796384475904,4.25095579577922,-10.8616689395862));
#23387=CARTESIAN_POINT('Ctrl Pts',(-2.26137136575613,4.17968274209439,-10.8672548790013));
#23388=CARTESIAN_POINT('Ctrl Pts',(-2.21608806072755,4.07473675640512,-10.8765467260252));
#23389=CARTESIAN_POINT('Ctrl Pts',(-2.2000930135488,4.04008256395551,-10.8797962235171));
#23390=CARTESIAN_POINT('Ctrl Pts',(-2.16628564461604,3.97143386483924,-10.8865780337264));
#23391=CARTESIAN_POINT('Ctrl Pts',(-2.14846743479671,3.93743084302305,-10.8901114717125));
#23392=CARTESIAN_POINT('Ctrl Pts',(-2.11100815043168,3.87012722042859,-10.897434898757));
#23393=CARTESIAN_POINT('Ctrl Pts',(-2.09129431600467,3.83672057611178,-10.9012383813503));
#23394=CARTESIAN_POINT('Ctrl Pts',(-2.05046094958217,3.77134095492018,-10.9089924865386));
#23395=CARTESIAN_POINT('Ctrl Pts',(-2.02926952283999,3.73923014273384,-10.9129573908145));
#23396=CARTESIAN_POINT('Ctrl Pts',(-1.98540346162804,3.67621926622253,-10.9210231443611));
#23397=CARTESIAN_POINT('Ctrl Pts',(-1.96272209651996,3.64530635015959,-10.92512534656));
#23398=CARTESIAN_POINT('Ctrl Pts',(-1.91587702393904,3.58465032601408,-10.9334375514149));
#23399=CARTESIAN_POINT('Ctrl Pts',(-1.89171329625648,3.5549072365286,-10.9376475756115));
#23400=CARTESIAN_POINT('Ctrl Pts',(-1.84190652454543,3.49658451455479,-10.9461451486341));
#23401=CARTESIAN_POINT('Ctrl Pts',(-1.81626348332508,3.46800488265077,-10.9504327184813));
#23402=CARTESIAN_POINT('Ctrl Pts',(-1.76349005078676,3.41201136675084,-10.9590552586289));
#23403=CARTESIAN_POINT('Ctrl Pts',(-1.7363596855068,3.38459746530546,-10.9633902505249));
#23404=CARTESIAN_POINT('Ctrl Pts',(-1.68059225573073,3.33094649266312,-10.972077285153));
#23405=CARTESIAN_POINT('Ctrl Pts',(-1.65195998582945,3.30471422081765,-10.976428573253));
#23406=CARTESIAN_POINT('Ctrl Pts',(-1.60784381620708,3.26624919219284,-10.9829473980705));
#23407=CARTESIAN_POINT('Ctrl Pts',(-1.59293142889825,3.25356637157806,-10.9851205633184));
#23408=CARTESIAN_POINT('Ctrl Pts',(-1.56287213526931,3.2286300328751,-10.9894373871103));
#23409=CARTESIAN_POINT('Ctrl Pts',(-1.54770701089334,3.21635854627108,-10.9915839288304));
#23410=CARTESIAN_POINT('Ctrl Pts',(-1.47124726535168,3.15602666933922,-11.0022410166242));
#23411=CARTESIAN_POINT('Ctrl Pts',(-1.40799822711262,3.11093266553086,-11.0105376568215));
#23412=CARTESIAN_POINT('Ctrl Pts',(-1.27743060091983,3.02697722307456,-11.0264485241274));
#23413=CARTESIAN_POINT('Ctrl Pts',(-1.21010900327941,2.98810844119082,-11.0340642433641));
#23414=CARTESIAN_POINT('Ctrl Pts',(-1.10603575631408,2.93449324692185,-11.0448165040961));
#23415=CARTESIAN_POINT('Ctrl Pts',(-1.07082872973356,2.91740410314997,-11.0482887604197));
#23416=CARTESIAN_POINT('Ctrl Pts',(-0.999365357715494,2.88481322043536,
-11.054982008906));
#23417=CARTESIAN_POINT('Ctrl Pts',(-0.963130129682714,2.8693200429042,-11.0582012189792));
#23418=CARTESIAN_POINT('Ctrl Pts',(-0.889500812844894,2.83992085997029,
-11.0643673298873));
#23419=CARTESIAN_POINT('Ctrl Pts',(-0.852281491609653,2.82609058473917,
-11.0672984223757));
#23420=CARTESIAN_POINT('Ctrl Pts',(-0.777480106558127,2.80031537803422,
-11.0728044734589));
#23421=CARTESIAN_POINT('Ctrl Pts',(-0.739808001792916,2.78833429109514,
-11.075387037792));
#23422=CARTESIAN_POINT('Ctrl Pts',(-0.626081142235231,2.75512486228593,
-11.0825926591987));
#23423=CARTESIAN_POINT('Ctrl Pts',(-0.549225020867577,2.73659502179654,
-11.0866800489708));
#23424=CARTESIAN_POINT('Ctrl Pts',(-0.432511795538508,2.714259073949,-11.0916421001459));
#23425=CARTESIAN_POINT('Ctrl Pts',(-0.39331219251049,2.7077195146796,-11.0931025310654));
#23426=CARTESIAN_POINT('Ctrl Pts',(-0.314496088528354,2.69649228340761,
-11.0956171788991));
#23427=CARTESIAN_POINT('Ctrl Pts',(-0.274695919596678,2.69178947522293,
-11.0966748018542));
#23428=CARTESIAN_POINT('Ctrl Pts',(-0.195299801987465,2.68432829145873,
-11.0983556871801));
#23429=CARTESIAN_POINT('Ctrl Pts',(-0.155652603752789,2.68155469534811,
-11.098982337027));
#23430=CARTESIAN_POINT('Ctrl Pts',(-0.0764579289352454,2.6778916390882,
-11.0998103951135));
#23431=CARTESIAN_POINT('Ctrl Pts',(-0.0369104896689312,2.67700143095427,
-11.1000119889358));
#23432=CARTESIAN_POINT('Ctrl Pts',(0.0815837784829221,2.67712330742632,
-11.0999843726987));
#23433=CARTESIAN_POINT('Ctrl Pts',(0.160382862315405,2.68092188458113,-11.0991228019287));
#23434=CARTESIAN_POINT('Ctrl Pts',(0.278286104013499,2.69219436339788,-11.0965837446232));
#23435=CARTESIAN_POINT('Ctrl Pts',(0.317537877518113,2.69688246104062,-11.0955295843832));
#23436=CARTESIAN_POINT('Ctrl Pts',(0.395941801212285,2.70814037681139,-11.0930084858397));
#23437=CARTESIAN_POINT('Ctrl Pts',(0.435094106484223,2.71471078980386,-11.0915413949138));
#23438=CARTESIAN_POINT('Ctrl Pts',(0.493746116159599,2.72600132427696,-11.0890336930226));
#23439=CARTESIAN_POINT('Ctrl Pts',(0.513309517811984,2.73001078199123,-11.0881451501855));
#23440=CARTESIAN_POINT('Ctrl Pts',(0.552256455133781,2.73847997335676,-11.086273564099));
#23441=CARTESIAN_POINT('Ctrl Pts',(0.571634753907634,2.74293742472352,-11.0852910185488));
#23442=CARTESIAN_POINT('Ctrl Pts',(0.629455063331992,2.75696591963619,-11.0822083735072));
#23443=CARTESIAN_POINT('Ctrl Pts',(0.667657542074438,2.76720614779721,-11.0799702944701));
#23444=CARTESIAN_POINT('Ctrl Pts',(0.781046169005456,2.80050386894502,-11.0727487414743));
#23445=CARTESIAN_POINT('Ctrl Pts',(0.855193468192384,2.82616680184042,-11.0672503698462));
#23446=CARTESIAN_POINT('Ctrl Pts',(0.964189026966947,2.86977153157994,-11.0581074024243));
#23447=CARTESIAN_POINT('Ctrl Pts',(1.00015468304478,2.88516068993715,-11.0549101944511));
#23448=CARTESIAN_POINT('Ctrl Pts',(1.07135197113703,2.91765546259803,-11.0482376006944));
#23449=CARTESIAN_POINT('Ctrl Pts',(1.1065836303793,2.93476100614121,-11.0447621885171));
#23450=CARTESIAN_POINT('Ctrl Pts',(1.17630609820376,2.97070906114556,-11.0375542330585));
#23451=CARTESIAN_POINT('Ctrl Pts',(1.2107826338078,2.98954328771685,-11.0338232927107));
#23452=CARTESIAN_POINT('Ctrl Pts',(1.27903955187267,3.02901587879235,-11.0261193965257));
#23453=CARTESIAN_POINT('Ctrl Pts',(1.31254945725883,3.04950014064211,-11.0221767713055));
#23454=CARTESIAN_POINT('Ctrl Pts',(1.37823901392251,3.09186099485949,-11.0141556229233));
#23455=CARTESIAN_POINT('Ctrl Pts',(1.41044151771734,3.11375084020812,-11.0100745081484));
#23456=CARTESIAN_POINT('Ctrl Pts',(1.47357760128402,3.15892606381394,-11.0018023721546));
#23457=CARTESIAN_POINT('Ctrl Pts',(1.50451216341957,3.1822121184455,-10.9976111942887));
#23458=CARTESIAN_POINT('Ctrl Pts',(1.59543396737852,3.2541520184694,-10.9849174124688));
#23459=CARTESIAN_POINT('Ctrl Pts',(1.65354585178342,3.3048853736236,-10.9762937510806));
#23460=CARTESIAN_POINT('Ctrl Pts',(1.73693817902585,3.38517496114059,-10.9632984167516));
#23461=CARTESIAN_POINT('Ctrl Pts',(1.76411205328141,3.41264540788295,-10.9589554791838));
#23462=CARTESIAN_POINT('Ctrl Pts',(1.81716937117498,3.46899272703761,-10.9502828043387));
#23463=CARTESIAN_POINT('Ctrl Pts',(1.84309667555061,3.49792107129187,-10.9459455511756));
#23464=CARTESIAN_POINT('Ctrl Pts',(1.89350371089981,3.55706432478315,-10.9373384473274));
#23465=CARTESIAN_POINT('Ctrl Pts',(1.91782002726333,3.58708091253443,-10.9330970558847));
#23466=CARTESIAN_POINT('Ctrl Pts',(1.96480545503627,3.64809681086166,-10.9247510204171));
#23467=CARTESIAN_POINT('Ctrl Pts',(1.98745910955116,3.67907795866426,-10.9206489900008));
#23468=CARTESIAN_POINT('Ctrl Pts',(2.05293600252221,3.77342700143773,-10.9085975966294));
#23469=CARTESIAN_POINT('Ctrl Pts',(2.09328053962265,3.83819748311837,-10.900902625416));
#23470=CARTESIAN_POINT('Ctrl Pts',(2.16737993193662,3.97149066954996,-10.8864120662151));
#23471=CARTESIAN_POINT('Ctrl Pts',(2.20113579376919,4.04002624499109,-10.8796157428706));
#23472=CARTESIAN_POINT('Ctrl Pts',(2.23910046262614,4.12808394712988,-10.8718244935691));
#23473=CARTESIAN_POINT('Ctrl Pts',(2.24648332267895,4.14582775641521,-10.8703010264556));
#23474=CARTESIAN_POINT('Ctrl Pts',(2.26081365706442,4.18153720245236,-10.8673296459906));
#23475=CARTESIAN_POINT('Ctrl Pts',(2.26777396396924,4.19954109715767,-10.865879022026));
#23476=CARTESIAN_POINT('Ctrl Pts',(2.28791485853621,4.25368668331467,-10.8616624914817));
#23477=CARTESIAN_POINT('Ctrl Pts',(2.30035376619681,4.28993814494949,-10.8590326047595));
#23478=CARTESIAN_POINT('Ctrl Pts',(2.32332083291499,4.36282874497073,-10.8541419345693));
#23479=CARTESIAN_POINT('Ctrl Pts',(2.33384408929083,4.39945372831524,-10.8518821742987));
#23480=CARTESIAN_POINT('Ctrl Pts',(2.35299205151236,4.4730596002693,-10.8477464746504));
#23481=CARTESIAN_POINT('Ctrl Pts',(2.36161668196543,4.51004050194072,-10.8458705231367));
#23482=CARTESIAN_POINT('Ctrl Pts',(2.38465480161393,4.62151562385937,-10.840837088678));
#23483=CARTESIAN_POINT('Ctrl Pts',(2.39623906502688,4.6965614004445,-10.8382739242991));
#23484=CARTESIAN_POINT('Ctrl Pts',(2.40787690299187,4.81014885074317,-10.8356921356679));
#23485=CARTESIAN_POINT('Ctrl Pts',(2.41079816467738,4.84822416052067,-10.8350420382505));
#23486=CARTESIAN_POINT('Ctrl Pts',(2.41371723344945,4.90556045584082,-10.8343919934576));
#23487=CARTESIAN_POINT('Ctrl Pts',(2.41444610176836,4.92472893436486,-10.8342295549678));
#23488=CARTESIAN_POINT('Ctrl Pts',(2.41541087362559,4.96315380364675,-10.8340145074147));
#23489=CARTESIAN_POINT('Ctrl Pts',(2.4156455512877,4.98241110455632,-10.8339621722294));
#23490=CARTESIAN_POINT('Ctrl Pts',(2.41560313911598,5.03999264903484,-10.833971630943));
#23491=CARTESIAN_POINT('Ctrl Pts',(2.4145875281457,5.07822847892658,-10.834198215873));
#23492=CARTESIAN_POINT('Ctrl Pts',(2.41061596210125,5.15440587986219,-10.835082583));
#23493=CARTESIAN_POINT('Ctrl Pts',(2.40766058078035,5.19234684080988,-10.8357402188351));
#23494=CARTESIAN_POINT('Ctrl Pts',(2.39592148041045,5.30573219765167,-10.8383441805306));
#23495=CARTESIAN_POINT('Ctrl Pts',(2.38427095852029,5.38073995810597,-10.8409216799096));
#23496=CARTESIAN_POINT('Ctrl Pts',(2.36107290737889,5.49238191222086,-10.8459889485252));
#23497=CARTESIAN_POINT('Ctrl Pts',(2.35238494926879,5.52945072166158,-10.8478782167291));
#23498=CARTESIAN_POINT('Ctrl Pts',(2.33307955313958,5.60329556878828,-10.8520466422376));
#23499=CARTESIAN_POINT('Ctrl Pts',(2.32246088539331,5.64007259006972,-10.8543260677788));
#23500=CARTESIAN_POINT('Ctrl Pts',(2.29926633375405,5.71332551677146,-10.8592630609384));
#23501=CARTESIAN_POINT('Ctrl Pts',(2.28665985543623,5.7498592815894,-10.8619268242372));
#23502=CARTESIAN_POINT('Ctrl Pts',(2.25978404179862,5.82174961553897,-10.8675499732185));
#23503=CARTESIAN_POINT('Ctrl Pts',(2.24546305066682,5.85727787033199,-10.8705204036662));
#23504=CARTESIAN_POINT('Ctrl Pts',(2.21511805933157,5.92741325183323,-10.8767444511339));
#23505=CARTESIAN_POINT('Ctrl Pts',(2.19908867693094,5.96203795192665,-10.8799992263874));
#23506=CARTESIAN_POINT('Ctrl Pts',(2.1653338515937,6.03041285824769,-10.8867673422212));
#23507=CARTESIAN_POINT('Ctrl Pts',(2.14760838564802,6.0641630512634,-10.8902807001735));
#23508=CARTESIAN_POINT('Ctrl Pts',(2.110466257554,6.13079395130041,-10.8975395078308));
#23509=CARTESIAN_POINT('Ctrl Pts',(2.09104959843572,6.16367465819078,-10.9012849744881));
#23510=CARTESIAN_POINT('Ctrl Pts',(2.05051737516466,6.2285652853405,-10.9089816490723));
#23511=CARTESIAN_POINT('Ctrl Pts',(2.02940184035635,6.26057521860074,-10.9129328744282));
#23512=CARTESIAN_POINT('Ctrl Pts',(1.98545129698501,6.32371657530621,-10.9210145348477));
#23513=CARTESIAN_POINT('Ctrl Pts',(1.96262998828763,6.35483019777428,-10.9251425458962));
#23514=CARTESIAN_POINT('Ctrl Pts',(1.91517913008013,6.41623574499544,-10.9335605156211));
#23515=CARTESIAN_POINT('Ctrl Pts',(1.89071033352914,6.44631744271524,-10.9378216781217));
#23516=CARTESIAN_POINT('Ctrl Pts',(1.8153924592825,6.53435906734782,-10.950662557146));
#23517=CARTESIAN_POINT('Ctrl Pts',(1.76248430705585,6.5903627060743,-10.9593285423635));
#23518=CARTESIAN_POINT('Ctrl Pts',(1.65143685751177,6.69700650572329,-10.9766108908935));
#23519=CARTESIAN_POINT('Ctrl Pts',(1.593287021374,6.74766692004806,-10.9852300851391));
#23520=CARTESIAN_POINT('Ctrl Pts',(1.47167902435032,6.84364147053686,-11.0021816610453));
#23521=CARTESIAN_POINT('Ctrl Pts',(1.40820021283237,6.88897017522776,-11.010517190463));
#23522=CARTESIAN_POINT('Ctrl Pts',(1.27579527666471,6.9740412210718,-11.0266436095859));
#23523=CARTESIAN_POINT('Ctrl Pts',(1.20797645046747,7.01307704737157,-11.0342982898015));
#23524=CARTESIAN_POINT('Ctrl Pts',(1.06908784663473,7.08445147588905,-11.048619592373));
#23525=CARTESIAN_POINT('Ctrl Pts',(0.998035979663791,7.11677742070683,-11.0552843505145));
#23526=CARTESIAN_POINT('Ctrl Pts',(0.852713243143896,7.17473256025119,-11.0674417000716));
#23527=CARTESIAN_POINT('Ctrl Pts',(0.778416648026101,7.20036362544414,-11.0729351492412));
#23528=CARTESIAN_POINT('Ctrl Pts',(0.664562228432768,7.23365210234308,-11.0801573497189));
#23529=CARTESIAN_POINT('Ctrl Pts',(0.626133503253441,7.24389773727957,-11.0823974328985));
#23530=CARTESIAN_POINT('Ctrl Pts',(0.548614559546499,7.26258443636509,-11.0865051926693));
#23531=CARTESIAN_POINT('Ctrl Pts',(0.509814499361565,7.2709566045556,-11.0883576190884));
#23532=CARTESIAN_POINT('Ctrl Pts',(0.431999673116113,7.28582934008303,-11.0916618070167));
#23533=CARTESIAN_POINT('Ctrl Pts',(0.393007691850147,7.29232444025252,-11.0931123766216));
#23534=CARTESIAN_POINT('Ctrl Pts',(0.314856544245277,7.30345579210369,-11.0956055483394));
#23535=CARTESIAN_POINT('Ctrl Pts',(0.275697371158881,7.30809196402797,-11.0966481564864));
#23536=CARTESIAN_POINT('Ctrl Pts',(0.157970235931856,7.3192272426051,-11.0991565661922));
#23537=CARTESIAN_POINT('Ctrl Pts',(0.0791383677753115,7.32295801741409,
-11.1000027737453));
#23538=CARTESIAN_POINT('Ctrl Pts',(3.59141650529373E-16,7.32295927629177,
-11.1000030851297));
#23539=CARTESIAN_POINT('Ctrl Pts',(4.03188655311423E-16,6.99999286992453,
-10.674155471012));
#23540=CARTESIAN_POINT('Ctrl Pts',(-0.0327607868253891,6.99999341185104,
-10.6741556207311));
#23541=CARTESIAN_POINT('Ctrl Pts',(-0.0656123585070314,6.9991872421877,
-10.6739517150638));
#23542=CARTESIAN_POINT('Ctrl Pts',(-0.114960332214575,6.99675429643007,
-10.6733374602853));
#23543=CARTESIAN_POINT('Ctrl Pts',(-0.131438158574352,6.99573753344068,
-10.6730808647556));
#23544=CARTESIAN_POINT('Ctrl Pts',(-0.164412953093731,6.99329215554895,
-10.6724643676842));
#23545=CARTESIAN_POINT('Ctrl Pts',(-0.180934362904284,6.99186054328014,
-10.6721037134189));
#23546=CARTESIAN_POINT('Ctrl Pts',(-0.230287429844603,6.98696511249956,
-10.670872066758));
#23547=CARTESIAN_POINT('Ctrl Pts',(-0.262963966116202,6.98290172605249,
-10.6698515754695));
#23548=CARTESIAN_POINT('Ctrl Pts',(-0.327908705561348,6.97320174713271,
-10.6674253892312));
#23549=CARTESIAN_POINT('Ctrl Pts',(-0.360171271143761,6.96756608870329,
-10.6660199372677));
#23550=CARTESIAN_POINT('Ctrl Pts',(-0.456338463152356,6.94833298322491,
-10.6612484953774));
#23551=CARTESIAN_POINT('Ctrl Pts',(-0.519623856019679,6.93241438830641,
-10.6573273498086));
#23552=CARTESIAN_POINT('Ctrl Pts',(-0.613321416348892,6.90390995199787,
-10.6504204814928));
#23553=CARTESIAN_POINT('Ctrl Pts',(-0.64434851851395,6.89363610314287,-10.6479472797978));
#23554=CARTESIAN_POINT('Ctrl Pts',(-0.705988882515448,6.87152937684899,
-10.6426732254099));
#23555=CARTESIAN_POINT('Ctrl Pts',(-0.736606669670444,6.85969376142734,
-10.6398717328137));
#23556=CARTESIAN_POINT('Ctrl Pts',(-0.797404453105115,6.83444903218893,
-10.6339578992176));
#23557=CARTESIAN_POINT('Ctrl Pts',(-0.827658932134272,6.82099820769395,
-10.6308362298514));
#23558=CARTESIAN_POINT('Ctrl Pts',(-0.887033500681286,6.7928238361157,-10.6243741050852));
#23559=CARTESIAN_POINT('Ctrl Pts',(-0.916289938854812,6.77804667454909,
-10.6210209859178));
#23560=CARTESIAN_POINT('Ctrl Pts',(-0.973878553221769,6.74716845091829,
-10.6141057400374));
#23561=CARTESIAN_POINT('Ctrl Pts',(-1.00222423052815,6.73106201891487,-10.6105423332443));
#23562=CARTESIAN_POINT('Ctrl Pts',(-1.0580299563462,6.69752805865601,-10.603230824273));
#23563=CARTESIAN_POINT('Ctrl Pts',(-1.0854899909806,6.6801005123873,-10.5994827019498));
#23564=CARTESIAN_POINT('Ctrl Pts',(-1.13952943376257,6.64392781924231,-10.5918282827977));
#23565=CARTESIAN_POINT('Ctrl Pts',(-1.16610884148417,6.62518267478179,-10.5879219662928));
#23566=CARTESIAN_POINT('Ctrl Pts',(-1.2183855857643,6.58636844771034,-10.5799777238751));
#23567=CARTESIAN_POINT('Ctrl Pts',(-1.24408293537336,6.56629938813905,-10.5759397777512));
#23568=CARTESIAN_POINT('Ctrl Pts',(-1.2945875598611,6.52482093459518,-10.5677592384192));
#23569=CARTESIAN_POINT('Ctrl Pts',(-1.31938405582187,6.50342102651133,-10.5636184501953));
#23570=CARTESIAN_POINT('Ctrl Pts',(-1.35593247228738,6.47026729747152,-10.5573441006669));
#23571=CARTESIAN_POINT('Ctrl Pts',(-1.3679974072164,6.4590479134576,-10.5552437152558));
#23572=CARTESIAN_POINT('Ctrl Pts',(-1.39176908071372,6.43638975092178,-10.5510504827809));
#23573=CARTESIAN_POINT('Ctrl Pts',(-1.40350118549718,6.42492924529715,-10.5489534246192));
#23574=CARTESIAN_POINT('Ctrl Pts',(-1.46131938383472,6.36703425868757,-10.5384876234438));
#23575=CARTESIAN_POINT('Ctrl Pts',(-1.50503629892909,6.31873216662301,-10.5301562291917));
#23576=CARTESIAN_POINT('Ctrl Pts',(-1.58746011044886,6.21826060242907,-10.5138160370322));
#23577=CARTESIAN_POINT('Ctrl Pts',(-1.6261773598651,6.16608565262814,-10.5058052968709));
#23578=CARTESIAN_POINT('Ctrl Pts',(-1.68049368448563,6.08488106269207,-10.4942020877408));
#23579=CARTESIAN_POINT('Ctrl Pts',(-1.6979715236584,6.05732173070268,-10.4904031348571));
#23580=CARTESIAN_POINT('Ctrl Pts',(-1.73165444174784,6.00120385596309,-10.4829727111617));
#23581=CARTESIAN_POINT('Ctrl Pts',(-1.74785206040866,5.97265941431339,-10.4793429259945));
#23582=CARTESIAN_POINT('Ctrl Pts',(-1.7789773120897,5.91449056577787,-10.4722747667905));
#23583=CARTESIAN_POINT('Ctrl Pts',(-1.79377941461961,5.88509622195569,-10.468864912625));
#23584=CARTESIAN_POINT('Ctrl Pts',(-1.82182423584976,5.82583025674177,-10.4623296155848));
#23585=CARTESIAN_POINT('Ctrl Pts',(-1.83508026493665,5.79593360600127,-10.4592011178087));
#23586=CARTESIAN_POINT('Ctrl Pts',(-1.87257263463879,5.70547680414255,-10.4502640856555));
#23587=CARTESIAN_POINT('Ctrl Pts',(-1.89454361314491,5.64414110197029,-10.4449026248875));
#23588=CARTESIAN_POINT('Ctrl Pts',(-1.92298482927188,5.55059537496581,-10.4378703784192));
#23589=CARTESIAN_POINT('Ctrl Pts',(-1.93171153527669,5.51915580674477,-10.4356945512933));
#23590=CARTESIAN_POINT('Ctrl Pts',(-1.94764437998263,5.45575588721916,-10.4316986913775));
#23591=CARTESIAN_POINT('Ctrl Pts',(-1.95485059856305,5.42379556319981,-10.4298786382116));
#23592=CARTESIAN_POINT('Ctrl Pts',(-1.96771811775107,5.35934497609858,-10.4266138899021));
#23593=CARTESIAN_POINT('Ctrl Pts',(-1.9733795127124,5.32685447536398,-10.4251691770077));
#23594=CARTESIAN_POINT('Ctrl Pts',(-1.98312038398174,5.26133125973539,-10.4226753014347));
#23595=CARTESIAN_POINT('Ctrl Pts',(-1.98715698321348,5.22858696432873,-10.4216371704946));
#23596=CARTESIAN_POINT('Ctrl Pts',(-1.99359803494776,5.16313102480355,-10.4199775228208));
#23597=CARTESIAN_POINT('Ctrl Pts',(-1.99600239898559,5.13041959628215,-10.4193560196127));
#23598=CARTESIAN_POINT('Ctrl Pts',(-1.9992013453422,5.06502938210275,-10.4185286163173));
#23599=CARTESIAN_POINT('Ctrl Pts',(-1.99999585293441,5.03235059790058,-10.4183227170519));
#23600=CARTESIAN_POINT('Ctrl Pts',(-1.99998069301495,4.93436289400731,-10.4183266750566));
#23601=CARTESIAN_POINT('Ctrl Pts',(-1.99677619101608,4.86909475106813,-10.4191586637422));
#23602=CARTESIAN_POINT('Ctrl Pts',(-1.98714366846619,4.77131374717008,-10.4216405774991));
#23603=CARTESIAN_POINT('Ctrl Pts',(-1.98312366864227,4.7387222380274,-10.422674438529));
#23604=CARTESIAN_POINT('Ctrl Pts',(-1.97587034821981,4.68988491866461,-10.4245314796529));
#23605=CARTESIAN_POINT('Ctrl Pts',(-1.97324571189318,4.67359979671702,-10.4252022714002));
#23606=CARTESIAN_POINT('Ctrl Pts',(-1.96758694588452,4.64105933331006,-10.4266450227394));
#23607=CARTESIAN_POINT('Ctrl Pts',(-1.96454580605742,4.62477030230104,-10.4274187572186));
#23608=CARTESIAN_POINT('Ctrl Pts',(-1.95483912128284,4.57613762972611,-10.4298815739684));
#23609=CARTESIAN_POINT('Ctrl Pts',(-1.94759760598414,4.5440349185319,-10.4317105123853));
#23610=CARTESIAN_POINT('Ctrl Pts',(-1.93159027695736,4.480384997727,-10.4357248708109));
#23611=CARTESIAN_POINT('Ctrl Pts',(-1.92282702673824,4.44884938566002,-10.437909636209));
#23612=CARTESIAN_POINT('Ctrl Pts',(-1.89428965717975,4.35509714570243,-10.444964928985));
#23613=CARTESIAN_POINT('Ctrl Pts',(-1.87227276296581,4.29373334968308,-10.4503365658497));
#23614=CARTESIAN_POINT('Ctrl Pts',(-1.83478104448698,4.20337824735948,-10.4592719345143));
#23615=CARTESIAN_POINT('Ctrl Pts',(-1.8215381549603,4.17354210751817,-10.4623967662073));
#23616=CARTESIAN_POINT('Ctrl Pts',(-1.79354778725739,4.11443779597759,-10.4689183947143));
#23617=CARTESIAN_POINT('Ctrl Pts',(-1.77879543413435,4.08516229300892,-10.4723162736268));
#23618=CARTESIAN_POINT('Ctrl Pts',(-1.74778151094684,4.02721604888781,-10.4793587400345));
#23619=CARTESIAN_POINT('Ctrl Pts',(-1.73145970029198,3.99845400767373,-10.4830163033902));
#23620=CARTESIAN_POINT('Ctrl Pts',(-1.69765225011823,3.94216426658589,-10.4904729251302));
#23621=CARTESIAN_POINT('Ctrl Pts',(-1.68010708628575,3.91451789496137,-10.4942857172838));
#23622=CARTESIAN_POINT('Ctrl Pts',(-1.64378875623639,3.86026756649618,-10.5020420311054));
#23623=CARTESIAN_POINT('Ctrl Pts',(-1.62501001747555,3.83365254472388,-10.5059868537968));
#23624=CARTESIAN_POINT('Ctrl Pts',(-1.58622525403486,3.78142966804803,-10.513980163911));
#23625=CARTESIAN_POINT('Ctrl Pts',(-1.56621921262261,3.75582182915573,-10.5180286720479));
#23626=CARTESIAN_POINT('Ctrl Pts',(-1.52498234923167,3.70560785024849,-10.526200238747));
#23627=CARTESIAN_POINT('Ctrl Pts',(-1.50375152957793,3.68100171073647,-10.5303233175237));
#23628=CARTESIAN_POINT('Ctrl Pts',(-1.46005845826469,3.63279310298997,-10.5386150570291));
#23629=CARTESIAN_POINT('Ctrl Pts',(-1.43759622816299,3.60919061973207,-10.5427837385248));
#23630=CARTESIAN_POINT('Ctrl Pts',(-1.39142431610491,3.56299886603047,-10.5511374982031));
#23631=CARTESIAN_POINT('Ctrl Pts',(-1.36771860377042,3.54041372767345,-10.5553218507049));
#23632=CARTESIAN_POINT('Ctrl Pts',(-1.33119319974296,3.5072965810337,-10.5615905831599));
#23633=CARTESIAN_POINT('Ctrl Pts',(-1.31884668425598,3.49637708233266,-10.563680375707));
#23634=CARTESIAN_POINT('Ctrl Pts',(-1.29395948634249,3.47490770053292,-10.5678315861114));
#23635=CARTESIAN_POINT('Ctrl Pts',(-1.28140372051583,3.46434234712297,-10.5698957765327));
#23636=CARTESIAN_POINT('Ctrl Pts',(-1.21809987701117,3.41239855072201,-10.580144008998));
#23637=CARTESIAN_POINT('Ctrl Pts',(-1.16573366535366,3.37357407066731,-10.5881223515868));
#23638=CARTESIAN_POINT('Ctrl Pts',(-1.05763191172308,3.30129114775118,-10.6034228042084));
#23639=CARTESIAN_POINT('Ctrl Pts',(-1.00189387792299,3.26782638260352,-10.6107463491238));
#23640=CARTESIAN_POINT('Ctrl Pts',(-0.915727798083462,3.2216654329248,-10.6210861032517));
#23641=CARTESIAN_POINT('Ctrl Pts',(-0.886578602188769,3.20695223237699,
-10.624425147714));
#23642=CARTESIAN_POINT('Ctrl Pts',(-0.827411440613592,3.17889253554151,
-10.6308616121367));
#23643=CARTESIAN_POINT('Ctrl Pts',(-0.797410958811738,3.16555341035283,
-10.6339573183767));
#23644=CARTESIAN_POINT('Ctrl Pts',(-0.73645053163076,3.14024166388806,-10.6398868686641));
#23645=CARTESIAN_POINT('Ctrl Pts',(-0.705635282768996,3.12833424384263,
-10.6427055108466));
#23646=CARTESIAN_POINT('Ctrl Pts',(-0.643704457082796,3.10614262380134,
-10.6480003242663));
#23647=CARTESIAN_POINT('Ctrl Pts',(-0.612514332036124,3.09582729511847,
-10.6504838094504));
#23648=CARTESIAN_POINT('Ctrl Pts',(-0.518355670264217,3.06723505008393,
-10.6574129897912));
#23649=CARTESIAN_POINT('Ctrl Pts',(-0.454723652597518,3.05128145621922,
-10.661343568329));
#23650=CARTESIAN_POINT('Ctrl Pts',(-0.358092468449763,3.03205092691298,
-10.666115252201));
#23651=CARTESIAN_POINT('Ctrl Pts',(-0.325637671252416,3.02642057770976,
-10.6675196542151));
#23652=CARTESIAN_POINT('Ctrl Pts',(-0.260382911681688,3.01675429439487,
-10.6699378284918));
#23653=CARTESIAN_POINT('Ctrl Pts',(-0.227430883820392,3.01270532852036,
-10.6709548761238));
#23654=CARTESIAN_POINT('Ctrl Pts',(-0.161695909574891,3.00628149040917,
-10.6725712748905));
#23655=CARTESIAN_POINT('Ctrl Pts',(-0.128870531795076,3.00389351378737,
-10.6731738835421));
#23656=CARTESIAN_POINT('Ctrl Pts',(-0.0633023394679634,3.00073974072009,
-10.6739701734787));
#23657=CARTESIAN_POINT('Ctrl Pts',(-0.0305595558175949,2.99997330028406,
-10.6741640332268));
#23658=CARTESIAN_POINT('Ctrl Pts',(0.067546219373333,3.00007823198808,-10.6741374764767));
#23659=CARTESIAN_POINT('Ctrl Pts',(0.132786887330565,3.0033486841664,-10.6733089595586));
#23660=CARTESIAN_POINT('Ctrl Pts',(0.230403329920755,3.01305392415495,-10.6708673122705));
#23661=CARTESIAN_POINT('Ctrl Pts',(0.262901320981579,3.0170902247284,-10.6698535945079));
#23662=CARTESIAN_POINT('Ctrl Pts',(0.327814821287288,3.0267829264048,-10.6674292170005));
#23663=CARTESIAN_POINT('Ctrl Pts',(0.360230458929732,3.0324398396669,-10.6660184104888));
#23664=CARTESIAN_POINT('Ctrl Pts',(0.408790621082765,3.04216062499209,-10.663606915676));
#23665=CARTESIAN_POINT('Ctrl Pts',(0.42498788289436,3.04561263851753,-10.6627524614643));
#23666=CARTESIAN_POINT('Ctrl Pts',(0.45723348883632,3.0529043385994,-10.6609526781029));
#23667=CARTESIAN_POINT('Ctrl Pts',(0.473277497147183,3.05674206018251,-10.6600078275582));
#23668=CARTESIAN_POINT('Ctrl Pts',(0.521149063986236,3.06882014096848,-10.6570434470816));
#23669=CARTESIAN_POINT('Ctrl Pts',(0.552778305210063,3.07763664649945,-10.6548912311395));
#23670=CARTESIAN_POINT('Ctrl Pts',(0.646656931716427,3.10630490838491,-10.6479467304191));
#23671=CARTESIAN_POINT('Ctrl Pts',(0.708046215587488,3.12839986430357,-10.6426593018352));
#23672=CARTESIAN_POINT('Ctrl Pts',(0.798287658930455,3.16594212751282,-10.6338671010601));
#23673=CARTESIAN_POINT('Ctrl Pts',(0.828064952167477,3.17919169555405,-10.6307925528174));
#23674=CARTESIAN_POINT('Ctrl Pts',(0.887011813046133,3.20716864473898,-10.6243759507131));
#23675=CARTESIAN_POINT('Ctrl Pts',(0.916181403230322,3.22189596496015,-10.6210338714703));
#23676=CARTESIAN_POINT('Ctrl Pts',(0.973907206011464,3.25284607864923,-10.6141024466226));
#23677=CARTESIAN_POINT('Ctrl Pts',(1.0024516014833,3.2690617390947,-10.6105146424553));
#23678=CARTESIAN_POINT('Ctrl Pts',(1.05896402156259,3.3030463644449,-10.6031063034683));
#23679=CARTESIAN_POINT('Ctrl Pts',(1.08670810822353,3.3206826519439,-10.5993149356424));
#23680=CARTESIAN_POINT('Ctrl Pts',(1.14109491510325,3.35715397852438,-10.5916015157244));
#23681=CARTESIAN_POINT('Ctrl Pts',(1.16775655576403,3.37600042799412,-10.5876769714456));
#23682=CARTESIAN_POINT('Ctrl Pts',(1.22002924808351,3.41489483567103,-10.579722192965));
#23683=CARTESIAN_POINT('Ctrl Pts',(1.24564111307727,3.43494337621453,-10.575691808126));
#23684=CARTESIAN_POINT('Ctrl Pts',(1.3209186281685,3.4968813053809,-10.5634850186665));
#23685=CARTESIAN_POINT('Ctrl Pts',(1.36903160068738,3.54056108470851,-10.5551922009365));
#23686=CARTESIAN_POINT('Ctrl Pts',(1.43807518428478,3.60968782498416,-10.542695427921));
#23687=CARTESIAN_POINT('Ctrl Pts',(1.46057343707218,3.63333899191555,-10.5385191055863));
#23688=CARTESIAN_POINT('Ctrl Pts',(1.50450154754197,3.68185221283114,-10.5301791547831));
#23689=CARTESIAN_POINT('Ctrl Pts',(1.52596771914682,3.70675858240798,-10.526008298773));
#23690=CARTESIAN_POINT('Ctrl Pts',(1.56770156294414,3.75767901243609,-10.5177314033589));
#23691=CARTESIAN_POINT('Ctrl Pts',(1.58783393815349,3.78352232449705,-10.5136527313689));
#23692=CARTESIAN_POINT('Ctrl Pts',(1.62673490683457,3.83605504121403,-10.5056268885413));
#23693=CARTESIAN_POINT('Ctrl Pts',(1.64549070297335,3.86272880830937,-10.501682231042));
#23694=CARTESIAN_POINT('Ctrl Pts',(1.69970143773757,3.94396028522575,-10.49009318503));
#23695=CARTESIAN_POINT('Ctrl Pts',(1.73310416808659,3.99972557688104,-10.4826934286111));
#23696=CARTESIAN_POINT('Ctrl Pts',(1.79445378809172,4.11448670299691,-10.4687587944868));
#23697=CARTESIAN_POINT('Ctrl Pts',(1.8224015111697,4.17349361871624,-10.462223209635));
#23698=CARTESIAN_POINT('Ctrl Pts',(1.85383386081593,4.24930845464478,-10.4547308688031));
#23699=CARTESIAN_POINT('Ctrl Pts',(1.85994640296646,4.26458530104584,-10.4532658489556));
#23700=CARTESIAN_POINT('Ctrl Pts',(1.87181101536952,4.29532998012479,-10.4504084644303));
#23701=CARTESIAN_POINT('Ctrl Pts',(1.87757371018256,4.31083075166611,-10.4490134931308));
#23702=CARTESIAN_POINT('Ctrl Pts',(1.89424909967874,4.35744835162015,-10.4449587282598));
#23703=CARTESIAN_POINT('Ctrl Pts',(1.90454773013222,4.3886596886135,-10.442429736193));
#23704=CARTESIAN_POINT('Ctrl Pts',(1.92356301179397,4.45141613975527,-10.4377266948003));
#23705=CARTESIAN_POINT('Ctrl Pts',(1.93227560389121,4.4829490668702,-10.4355536294173));
#23706=CARTESIAN_POINT('Ctrl Pts',(1.94812890807492,4.54632134403188,-10.4315765943941));
#23707=CARTESIAN_POINT('Ctrl Pts',(1.95526955774118,4.57816070532523,-10.4297726130834));
#23708=CARTESIAN_POINT('Ctrl Pts',(1.97434366674437,4.67413718295142,-10.424932284522));
#23709=CARTESIAN_POINT('Ctrl Pts',(1.98393470570248,4.7387491714715,-10.4224674550198));
#23710=CARTESIAN_POINT('Ctrl Pts',(1.99357010100791,4.836544295573,-10.4199847157782));
#23711=CARTESIAN_POINT('Ctrl Pts',(1.99598872130629,4.86932590687989,-10.4193595591137));
#23712=CARTESIAN_POINT('Ctrl Pts',(1.99840552601066,4.91869060431424,-10.4187344530547));
#23713=CARTESIAN_POINT('Ctrl Pts',(1.99900898297575,4.93519404488994,-10.4185782464589));
#23714=CARTESIAN_POINT('Ctrl Pts',(1.99980775318135,4.96827661563313,-10.4183714491277));
#23715=CARTESIAN_POINT('Ctrl Pts',(2.00000205147375,4.98485652941228,-10.4183211217629));
#23716=CARTESIAN_POINT('Ctrl Pts',(1.99996693687244,5.03443237844717,-10.4183302175963));
#23717=CARTESIAN_POINT('Ctrl Pts',(1.99912607508997,5.06735219238454,-10.4185481096773));
#23718=CARTESIAN_POINT('Ctrl Pts',(1.99583786907306,5.13293847289988,-10.4193985483784));
#23719=CARTESIAN_POINT('Ctrl Pts',(1.99339099987005,5.16560441420555,-10.420030954252));
#23720=CARTESIAN_POINT('Ctrl Pts',(1.98367176568468,5.26322554237064,-10.4225350158964));
#23721=CARTESIAN_POINT('Ctrl Pts',(1.97402586888932,5.32780480023109,-10.4250136304415));
#23722=CARTESIAN_POINT('Ctrl Pts',(1.9548193467042,5.42392491498701,-10.4298864951246));
#23723=CARTESIAN_POINT('Ctrl Pts',(1.94762626573488,5.45583996202888,-10.4317032822354));
#23724=CARTESIAN_POINT('Ctrl Pts',(1.93164261621215,5.51941798909179,-10.4357117876031));
#23725=CARTESIAN_POINT('Ctrl Pts',(1.92285102952203,5.55108181595763,-10.4379037638056));
#23726=CARTESIAN_POINT('Ctrl Pts',(1.90364740470372,5.61415021866191,-10.4426513510036));
#23727=CARTESIAN_POINT('Ctrl Pts',(1.89321003632208,5.6456046095741,-10.4452129199845));
#23728=CARTESIAN_POINT('Ctrl Pts',(1.87095855891445,5.70749986395087,-10.4506203388836));
#23729=CARTESIAN_POINT('Ctrl Pts',(1.85910168213551,5.73808854322452,-10.4534768098387));
#23730=CARTESIAN_POINT('Ctrl Pts',(1.8339779445532,5.79847284025612,-10.4594620739706));
#23731=CARTESIAN_POINT('Ctrl Pts',(1.82070662763005,5.82828358813145,-10.4625919809456));
#23732=CARTESIAN_POINT('Ctrl Pts',(1.79275976270791,5.88715217292303,-10.469100440457));
#23733=CARTESIAN_POINT('Ctrl Pts',(1.77808419565885,5.91620999846434,-10.4724790096989));
#23734=CARTESIAN_POINT('Ctrl Pts',(1.74733285784584,5.9735770502033,-10.479459335819));
#23735=CARTESIAN_POINT('Ctrl Pts',(1.73125708959058,6.00188627628834,-10.4830611089991));
#23736=CARTESIAN_POINT('Ctrl Pts',(1.69769896693899,6.05775500930874,-10.4904625034394));
#23737=CARTESIAN_POINT('Ctrl Pts',(1.680216636838,6.08531452743744,-10.4942621414599));
#23738=CARTESIAN_POINT('Ctrl Pts',(1.6438283608928,6.13967719513339,-10.5020337518928));
#23739=CARTESIAN_POINT('Ctrl Pts',(1.62493375767266,6.16646501863456,-10.5060033932866));
#23740=CARTESIAN_POINT('Ctrl Pts',(1.58564744196769,6.21933321045759,-10.5140984106397));
#23741=CARTESIAN_POINT('Ctrl Pts',(1.56538882278599,6.24523258009862,-10.5181960951784));
#23742=CARTESIAN_POINT('Ctrl Pts',(1.50303037664793,6.32103357381821,-10.5305443385106));
#23743=CARTESIAN_POINT('Ctrl Pts',(1.45922576593362,6.36925089699378,-10.5388778563317));
#23744=CARTESIAN_POINT('Ctrl Pts',(1.36728548654099,6.4610677622726,-10.5554971737949));
#23745=CARTESIAN_POINT('Ctrl Pts',(1.31914109238269,6.50468474190315,-10.5637856957625));
#23746=CARTESIAN_POINT('Ctrl Pts',(1.21845734621205,6.58731572843475,-10.5800869305743));
#23747=CARTESIAN_POINT('Ctrl Pts',(1.16590089678122,6.62634227836551,-10.5881026704127));
#23748=CARTESIAN_POINT('Ctrl Pts',(1.05627796645429,6.69958569974766,-10.6036104052836));
#23749=CARTESIAN_POINT('Ctrl Pts',(1.00012825879239,6.73319428473922,-10.610971416454));
#23750=CARTESIAN_POINT('Ctrl Pts',(0.885137260859031,6.79464536121258,-10.6247432874189));
#23751=CARTESIAN_POINT('Ctrl Pts',(0.826310799492401,6.82247695507946,-10.6311523545183));
#23752=CARTESIAN_POINT('Ctrl Pts',(0.705992745787938,6.8723744573944,-10.6428432917456));
#23753=CARTESIAN_POINT('Ctrl Pts',(0.644479854326622,6.89444197624564,-10.648125986718));
#23754=CARTESIAN_POINT('Ctrl Pts',(0.550215580868819,6.92310227913939,-10.6550711100818));
#23755=CARTESIAN_POINT('Ctrl Pts',(0.518399021882904,6.93192343972681,-10.6572252532775));
#23756=CARTESIAN_POINT('Ctrl Pts',(0.454218229150574,6.94801208377446,-10.6611754203266));
#23757=CARTESIAN_POINT('Ctrl Pts',(0.422094228207732,6.95522025003796,-10.6629567790744));
#23758=CARTESIAN_POINT('Ctrl Pts',(0.357668463408306,6.96802519471123,-10.6661342030247));
#23759=CARTESIAN_POINT('Ctrl Pts',(0.325385563923601,6.97361726606649,-10.6675291220501));
#23760=CARTESIAN_POINT('Ctrl Pts',(0.260681346265714,6.98320100029813,-10.6699266441343));
#23761=CARTESIAN_POINT('Ctrl Pts',(0.228260022506622,6.98719259450597,-10.6709292529959));
#23762=CARTESIAN_POINT('Ctrl Pts',(0.130789384959454,6.99677970952189,-10.6733414284682));
#23763=CARTESIAN_POINT('Ctrl Pts',(0.0655215736507795,6.99999178607152,
-10.6741551715738));
#23764=CARTESIAN_POINT('Ctrl Pts',(4.03188655311423E-16,6.99999286992453,
-10.674155471012));
#23765=CARTESIAN_POINT('Ctrl Pts',(5.66553889764798E-16,7.,-10.6741648723787));
#23766=CARTESIAN_POINT('Ctrl Pts',(3.59143153197828E-16,7.32295693650353,
-11.1));
#23767=CARTESIAN_POINT('Origin',(0.,274.500012,0.));
#23768=CARTESIAN_POINT('',(-1.12667505521557E-15,274.500012,-9.2));
#23769=CARTESIAN_POINT('Origin',(0.,0.,0.));
#23770=CARTESIAN_POINT('',(-1.18790739517294E-15,0.,9.70000000000007));
#23771=CARTESIAN_POINT('Origin',(0.,275.,0.));
#23772=CARTESIAN_POINT('',(-1.2981256070962E-15,275.,10.6));
#23773=CARTESIAN_POINT('Origin',(0.,0.499999999999945,0.));
#23774=CARTESIAN_POINT('',(-1.35935794705356E-15,0.499999999999945,-11.1));
#23775=CARTESIAN_POINT('',(0.,0.,0.));
#23776=CARTESIAN_POINT('Origin',(0.,10.,0.));
#23777=CARTESIAN_POINT('',(0.,0.,9.1));
#23778=CARTESIAN_POINT('Origin',(0.,0.,0.));
#23779=CARTESIAN_POINT('',(-4.87825354572973E-16,2.875,9.1));
#23780=CARTESIAN_POINT('',(-1.11442858722409E-15,10.,9.1));
#23781=CARTESIAN_POINT('',(-2.125,5.,8.84841087427567));
#23782=CARTESIAN_POINT('Ctrl Pts',(1.38777878078145E-16,2.875,9.1));
#23783=CARTESIAN_POINT('Ctrl Pts',(-0.267873575081806,2.875,9.1));
#23784=CARTESIAN_POINT('Ctrl Pts',(-0.5529354090087,2.92873648721047,9.08698350329319));
#23785=CARTESIAN_POINT('Ctrl Pts',(-1.07620906803504,3.145911519284,9.03995469026056));
#23786=CARTESIAN_POINT('Ctrl Pts',(-1.31450018724633,3.3092963672035,9.00657888722713));
#23787=CARTESIAN_POINT('Ctrl Pts',(-1.69072350014861,3.68551968010578,8.94359188045991));
#23788=CARTESIAN_POINT('Ctrl Pts',(-1.85409283030911,3.92380246738359,8.9098094730266));
#23789=CARTESIAN_POINT('Ctrl Pts',(-2.0712565629818,4.44704679048386,8.86184301458953));
#23790=CARTESIAN_POINT('Ctrl Pts',(-2.125,4.73209813204263,8.84841087427567));
#23791=CARTESIAN_POINT('Ctrl Pts',(-2.125,5.,8.84841087427567));
#23792=CARTESIAN_POINT('',(-5.2251982409251E-16,7.125,9.1));
#23793=CARTESIAN_POINT('Ctrl Pts',(-2.125,5.,8.84841087427567));
#23794=CARTESIAN_POINT('Ctrl Pts',(-2.125,5.26790186795737,8.84841087427567));
#23795=CARTESIAN_POINT('Ctrl Pts',(-2.0712565629818,5.55295320951614,8.86184301458953));
#23796=CARTESIAN_POINT('Ctrl Pts',(-1.85409283030911,6.07619753261641,8.9098094730266));
#23797=CARTESIAN_POINT('Ctrl Pts',(-1.69072350014861,6.31448031989422,8.94359188045991));
#23798=CARTESIAN_POINT('Ctrl Pts',(-1.31450018724633,6.6907036327965,9.00657888722713));
#23799=CARTESIAN_POINT('Ctrl Pts',(-1.07620906803504,6.854088480716,9.03995469026056));
#23800=CARTESIAN_POINT('Ctrl Pts',(-0.552935409008698,7.07126351278953,
9.08698350329319));
#23801=CARTESIAN_POINT('Ctrl Pts',(-0.267873575081805,7.125,9.1));
#23802=CARTESIAN_POINT('Ctrl Pts',(3.46944695195361E-16,7.125,9.1));
#23803=CARTESIAN_POINT('',(0.,10.,9.1));
#23804=CARTESIAN_POINT('',(-1.11442858722409E-15,10.,9.1));
#23805=CARTESIAN_POINT('Origin',(0.,10.,0.));
#23806=CARTESIAN_POINT('',(2.125,5.,8.84841087427567));
#23807=CARTESIAN_POINT('Ctrl Pts',(2.77555756156289E-16,7.125,9.1));
#23808=CARTESIAN_POINT('Ctrl Pts',(0.267873575081806,7.125,9.1));
#23809=CARTESIAN_POINT('Ctrl Pts',(0.5529354090087,7.07126351278953,9.08698350329319));
#23810=CARTESIAN_POINT('Ctrl Pts',(1.07620906803504,6.854088480716,9.03995469026056));
#23811=CARTESIAN_POINT('Ctrl Pts',(1.31450018724633,6.6907036327965,9.00657888722713));
#23812=CARTESIAN_POINT('Ctrl Pts',(1.69072350014861,6.31448031989422,8.94359188045991));
#23813=CARTESIAN_POINT('Ctrl Pts',(1.85409283030911,6.07619753261641,8.9098094730266));
#23814=CARTESIAN_POINT('Ctrl Pts',(2.0712565629818,5.55295320951614,8.86184301458953));
#23815=CARTESIAN_POINT('Ctrl Pts',(2.125,5.26790186795737,8.84841087427567));
#23816=CARTESIAN_POINT('Ctrl Pts',(2.125,5.,8.84841087427567));
#23817=CARTESIAN_POINT('Ctrl Pts',(2.125,5.,8.84841087427567));
#23818=CARTESIAN_POINT('Ctrl Pts',(2.125,4.73209813204263,8.84841087427567));
#23819=CARTESIAN_POINT('Ctrl Pts',(2.0712565629818,4.44704679048386,8.86184301458953));
#23820=CARTESIAN_POINT('Ctrl Pts',(1.85409283030911,3.92380246738359,8.9098094730266));
#23821=CARTESIAN_POINT('Ctrl Pts',(1.69072350014861,3.68551968010578,8.94359188045991));
#23822=CARTESIAN_POINT('Ctrl Pts',(1.31450018724633,3.3092963672035,9.00657888722713));
#23823=CARTESIAN_POINT('Ctrl Pts',(1.07620906803504,3.145911519284,9.03995469026056));
#23824=CARTESIAN_POINT('Ctrl Pts',(0.552935409008699,2.92873648721047,9.08698350329319));
#23825=CARTESIAN_POINT('Ctrl Pts',(0.267873575081806,2.875,9.1));
#23826=CARTESIAN_POINT('Ctrl Pts',(1.38777878078145E-16,2.875,9.1));
#23827=CARTESIAN_POINT('',(0.,7.125,-9.1));
#23828=CARTESIAN_POINT('',(2.125,5.,-8.84841087427567));
#23829=CARTESIAN_POINT('Ctrl Pts',(-1.38777878078145E-16,7.125,-9.1));
#23830=CARTESIAN_POINT('Ctrl Pts',(0.267873575081805,7.125,-9.1));
#23831=CARTESIAN_POINT('Ctrl Pts',(0.552935409008698,7.07126351278953,-9.08698350329319));
#23832=CARTESIAN_POINT('Ctrl Pts',(1.07620906803504,6.854088480716,-9.03995469026056));
#23833=CARTESIAN_POINT('Ctrl Pts',(1.31450018724633,6.6907036327965,-9.00657888722713));
#23834=CARTESIAN_POINT('Ctrl Pts',(1.69072350014861,6.31448031989422,-8.94359188045991));
#23835=CARTESIAN_POINT('Ctrl Pts',(1.85409283030911,6.07619753261641,-8.9098094730266));
#23836=CARTESIAN_POINT('Ctrl Pts',(2.0712565629818,5.55295320951614,-8.86184301458953));
#23837=CARTESIAN_POINT('Ctrl Pts',(2.125,5.26790186795737,-8.84841087427567));
#23838=CARTESIAN_POINT('Ctrl Pts',(2.125,5.,-8.84841087427567));
#23839=CARTESIAN_POINT('Ctrl Pts',(2.125,5.,-8.84841087427567));
#23840=CARTESIAN_POINT('Ctrl Pts',(2.125,4.73209813204263,-8.84841087427567));
#23841=CARTESIAN_POINT('Ctrl Pts',(2.0712565629818,4.44704679048386,-8.86184301458953));
#23842=CARTESIAN_POINT('Ctrl Pts',(1.85409283030911,3.92380246738359,-8.9098094730266));
#23843=CARTESIAN_POINT('Ctrl Pts',(1.69072350014861,3.68551968010578,-8.94359188045991));
#23844=CARTESIAN_POINT('Ctrl Pts',(1.31450018724633,3.3092963672035,-9.00657888722713));
#23845=CARTESIAN_POINT('Ctrl Pts',(1.07620906803504,3.145911519284,-9.03995469026056));
#23846=CARTESIAN_POINT('Ctrl Pts',(0.5529354090087,2.92873648721047,-9.08698350329319));
#23847=CARTESIAN_POINT('Ctrl Pts',(0.267873575081805,2.875,-9.1));
#23848=CARTESIAN_POINT('Ctrl Pts',(-0.267873575081806,2.875,-9.1));
#23849=CARTESIAN_POINT('Ctrl Pts',(-0.552935409008699,2.92873648721047,
-9.08698350329319));
#23850=CARTESIAN_POINT('Ctrl Pts',(-1.07620906803504,3.145911519284,-9.03995469026056));
#23851=CARTESIAN_POINT('Ctrl Pts',(-1.31450018724633,3.3092963672035,-9.00657888722713));
#23852=CARTESIAN_POINT('Ctrl Pts',(-1.69072350014861,3.68551968010578,-8.94359188045991));
#23853=CARTESIAN_POINT('Ctrl Pts',(-1.85409283030911,3.92380246738359,-8.9098094730266));
#23854=CARTESIAN_POINT('Ctrl Pts',(-2.0712565629818,4.44704679048386,-8.86184301458953));
#23855=CARTESIAN_POINT('Ctrl Pts',(-2.125,4.73209813204263,-8.84841087427567));
#23856=CARTESIAN_POINT('Ctrl Pts',(-2.125,5.26790186795737,-8.84841087427567));
#23857=CARTESIAN_POINT('Ctrl Pts',(-2.0712565629818,5.55295320951614,-8.86184301458953));
#23858=CARTESIAN_POINT('Ctrl Pts',(-1.85409283030911,6.07619753261641,-8.9098094730266));
#23859=CARTESIAN_POINT('Ctrl Pts',(-1.69072350014861,6.31448031989422,-8.94359188045991));
#23860=CARTESIAN_POINT('Ctrl Pts',(-1.31450018724633,6.6907036327965,-9.00657888722713));
#23861=CARTESIAN_POINT('Ctrl Pts',(-1.07620906803504,6.854088480716,-9.03995469026056));
#23862=CARTESIAN_POINT('Ctrl Pts',(-0.5529354090087,7.07126351278953,-9.08698350329319));
#23863=CARTESIAN_POINT('Ctrl Pts',(-0.267873575081806,7.125,-9.1));
#23864=CARTESIAN_POINT('Ctrl Pts',(-2.08166817117217E-16,7.125,-9.1));
#23865=CARTESIAN_POINT('Origin',(0.,10.,0.));
#23866=CARTESIAN_POINT('',(0.,10.,3.5));
#23867=CARTESIAN_POINT('Origin',(0.,10.,0.));
#23868=CARTESIAN_POINT('Origin',(0.,0.,0.));
#23869=CARTESIAN_POINT('',(-4.28626379701573E-16,1.22464679914735E-16,3.5));
#23870=CARTESIAN_POINT('Origin',(0.,1.22464679914735E-16,0.));
#23871=CARTESIAN_POINT('Origin',(0.,5.,6.1));
#23872=CARTESIAN_POINT('',(-2.125,5.,6.1));
#23873=CARTESIAN_POINT('Origin',(0.,5.,6.1));
#23874=CARTESIAN_POINT('',(-2.125,5.,6.1));
#23875=CARTESIAN_POINT('Origin',(0.,5.,6.1));
#23876=CARTESIAN_POINT('Origin',(0.,5.,-6.1));
#23877=CARTESIAN_POINT('',(2.125,5.,-6.1));
#23878=CARTESIAN_POINT('Origin',(0.,5.,-6.1));
#23879=CARTESIAN_POINT('',(2.125,5.,-6.1));
#23880=CARTESIAN_POINT('Origin',(0.,5.,-6.1));
#23881=CARTESIAN_POINT('Origin',(0.,0.,0.));
#23882=CARTESIAN_POINT('',(-4.28626379701573E-16,0.,3.5));
#23883=CARTESIAN_POINT('',(0.,0.,0.));
#23884=CARTESIAN_POINT('Origin',(-5.,74.6,0.));
#23885=CARTESIAN_POINT('',(-6.12323399573677E-16,74.6,5.));
#23886=CARTESIAN_POINT('Origin',(0.,74.6,0.));
#23887=CARTESIAN_POINT('',(-3.67394039744206E-16,74.6,-3.));
#23888=CARTESIAN_POINT('Origin',(0.,74.6,0.));
#23889=CARTESIAN_POINT('Origin',(0.,0.,0.));
#23890=CARTESIAN_POINT('',(-6.12323399573677E-16,76.5,5.));
#23891=CARTESIAN_POINT('',(-6.12323399573677E-16,0.,5.));
#23892=CARTESIAN_POINT('Origin',(0.,76.5,0.));
#23893=CARTESIAN_POINT('Origin',(-1.75,77.,0.));
#23894=CARTESIAN_POINT('',(-5.51091059616309E-16,77.,4.5));
#23895=CARTESIAN_POINT('Origin',(0.,77.,0.));
#23896=CARTESIAN_POINT('',(2.14313189850787E-16,77.,1.75));
#23897=CARTESIAN_POINT('Origin',(0.,77.,0.));
#23898=CARTESIAN_POINT('Origin',(0.,77.,0.));
#23899=CARTESIAN_POINT('',(1.31228980982913E-32,78.75,1.07156594925393E-16));
#23900=CARTESIAN_POINT('Origin',(0.,77.,0.));
#23901=CARTESIAN_POINT('Origin',(0.,76.5,0.));
#23902=CARTESIAN_POINT('Origin',(-5.51091059616309E-16,76.5,4.5));
#23903=CARTESIAN_POINT('Origin',(0.,0.,0.));
#23904=CARTESIAN_POINT('',(-3.67394039744206E-16,0.554499999999991,-3.));
#23905=CARTESIAN_POINT('',(-3.67394039744206E-16,0.,-3.));
#23906=CARTESIAN_POINT('Origin',(0.,0.554499999999991,0.));
#23907=CARTESIAN_POINT('Origin',(0.,0.,0.));
#23908=CARTESIAN_POINT('',(-2.99487374731485E-16,-3.66766254849957E-32,
-2.4455));
#23909=CARTESIAN_POINT('',(-2.99487374731485E-16,0.,-2.4455));
#23910=CARTESIAN_POINT('Origin',(0.,0.,0.));
#23911=CARTESIAN_POINT('Origin',(0.,4.5,0.));
#23912=CARTESIAN_POINT('',(2.,4.5,1.15470053837925));
#23913=CARTESIAN_POINT('',(4.86323526963846E-16,4.5,2.3094010767585));
#23914=CARTESIAN_POINT('',(2.,4.5,1.15470053837925));
#23915=CARTESIAN_POINT('',(-2.,4.5,1.15470053837925));
#23916=CARTESIAN_POINT('',(4.86323526963846E-16,4.5,2.3094010767585));
#23917=CARTESIAN_POINT('',(-2.,4.5,-1.15470053837925));
#23918=CARTESIAN_POINT('',(-2.,4.5,1.15470053837925));
#23919=CARTESIAN_POINT('',(2.07283766416844E-16,4.5,-2.3094010767585));
#23920=CARTESIAN_POINT('',(-2.,4.5,-1.15470053837925));
#23921=CARTESIAN_POINT('',(2.,4.5,-1.15470053837925));
#23922=CARTESIAN_POINT('',(2.07283766416844E-16,4.5,-2.3094010767585));
#23923=CARTESIAN_POINT('',(2.,4.5,-1.15470053837925));
#23924=CARTESIAN_POINT('Origin',(-2.,4.5,1.15470053837925));
#23925=CARTESIAN_POINT('',(-2.,0.,1.15470053837925));
#23926=CARTESIAN_POINT('',(-2.,0.,-1.15470053837925));
#23927=CARTESIAN_POINT('',(-2.,0.,1.15470053837925));
#23928=CARTESIAN_POINT('',(-2.,4.5,-1.15470053837925));
#23929=CARTESIAN_POINT('',(-2.,4.5,1.15470053837925));
#23930=CARTESIAN_POINT('Origin',(-2.,4.5,-1.15470053837925));
#23931=CARTESIAN_POINT('',(2.07283766416844E-16,0.,-2.3094010767585));
#23932=CARTESIAN_POINT('',(-2.,0.,-1.15470053837925));
#23933=CARTESIAN_POINT('',(2.07283766416844E-16,4.5,-2.3094010767585));
#23934=CARTESIAN_POINT('Origin',(2.07283766416844E-16,4.5,-2.3094010767585));
#23935=CARTESIAN_POINT('',(2.,0.,-1.15470053837925));
#23936=CARTESIAN_POINT('',(2.07283766416844E-16,0.,-2.3094010767585));
#23937=CARTESIAN_POINT('',(2.,4.5,-1.15470053837925));
#23938=CARTESIAN_POINT('Origin',(2.,4.5,-1.15470053837925));
#23939=CARTESIAN_POINT('',(2.,0.,1.15470053837925));
#23940=CARTESIAN_POINT('',(2.,0.,-1.15470053837925));
#23941=CARTESIAN_POINT('',(2.,4.5,1.15470053837925));
#23942=CARTESIAN_POINT('Origin',(2.,4.5,1.15470053837925));
#23943=CARTESIAN_POINT('',(8.67361737988404E-16,0.,2.3094010767585));
#23944=CARTESIAN_POINT('',(2.,0.,1.15470053837925));
#23945=CARTESIAN_POINT('',(4.86323526963846E-16,4.5,2.3094010767585));
#23946=CARTESIAN_POINT('Origin',(4.86323526963846E-16,4.5,2.3094010767585));
#23947=CARTESIAN_POINT('',(4.86323526963846E-16,0.,2.3094010767585));
#23948=CARTESIAN_POINT('Origin',(-3.49999999999999,0.,0.));
#23949=CARTESIAN_POINT('',(0.,0.,0.));
#23950=CARTESIAN_POINT('Origin',(5.54667823983524E-29,0.,9.29999999999998));
#23951=CARTESIAN_POINT('',(2.77333911991762E-29,0.,5.29999999999999));
#23952=CARTESIAN_POINT('',(5.54667823983524E-29,0.,9.29999999999998));
#23953=CARTESIAN_POINT('Origin',(4.16000867987643E-29,0.,7.29999999999999));
#23954=CARTESIAN_POINT('',(5.54667823983524E-29,0.,9.29999999999998));
#23955=CARTESIAN_POINT('Origin',(1.03537993810258E-27,90.,9.29999999999998));
#23956=CARTESIAN_POINT('',(1.01689101063646E-27,90.,5.3));
#23957=CARTESIAN_POINT('',(1.03537993810258E-27,90.,9.29999999999998));
#23958=CARTESIAN_POINT('',(1.03537993810258E-27,90.,9.29999999999998));
#23959=CARTESIAN_POINT('Origin',(1.02613547436952E-27,90.,7.3));
#23960=CARTESIAN_POINT('Ctrl Pts',(2.77333911991762E-29,0.,5.29999999999999));
#23961=CARTESIAN_POINT('Ctrl Pts',(-1.42013071988495,0.197368421052638,
5.29999999999998));
#23962=CARTESIAN_POINT('Ctrl Pts',(-2.65,0.394736842105281,4.58993464005751));
#23963=CARTESIAN_POINT('Ctrl Pts',(-3.87986928011504,0.592105263157915,
3.87986928011505));
#23964=CARTESIAN_POINT('Ctrl Pts',(-4.58993464005751,0.789473684210562,
2.65));
#23965=CARTESIAN_POINT('Ctrl Pts',(-5.29999999999999,0.986842105263191,
1.42013071988495));
#23966=CARTESIAN_POINT('Ctrl Pts',(-5.29999999999999,1.18421052631579,3.24531401774024E-16));
#23967=CARTESIAN_POINT('Ctrl Pts',(-5.29999999999999,1.38157894736841,-1.42013071988495));
#23968=CARTESIAN_POINT('Ctrl Pts',(-4.58993464005751,1.57894736842107,-2.64999999999999));
#23969=CARTESIAN_POINT('Ctrl Pts',(-3.87986928011504,1.77631578947369,-3.87986928011504));
#23970=CARTESIAN_POINT('Ctrl Pts',(-2.65,1.97368421052629,-4.58993464005751));
#23971=CARTESIAN_POINT('Ctrl Pts',(-1.42013071988495,2.17105263157891,-5.29999999999999));
#23972=CARTESIAN_POINT('Ctrl Pts',(-6.49062803548097E-16,2.36842105263158,
-5.29999999999999));
#23973=CARTESIAN_POINT('Ctrl Pts',(1.42013071988495,2.56578947368418,-5.29999999999999));
#23974=CARTESIAN_POINT('Ctrl Pts',(2.64999999999999,2.7631578947368,-4.58993464005751));
#23975=CARTESIAN_POINT('Ctrl Pts',(3.87986928011504,2.96052631578946,-3.87986928011505));
#23976=CARTESIAN_POINT('Ctrl Pts',(4.58993464005751,3.15789473684208,-2.65));
#23977=CARTESIAN_POINT('Ctrl Pts',(5.29999999999999,3.35526315789473,-1.42013071988495));
#23978=CARTESIAN_POINT('Ctrl Pts',(5.29999999999999,3.55263157894736,-9.73594205321085E-16));
#23979=CARTESIAN_POINT('Ctrl Pts',(5.29999999999999,3.75000000000001,1.42013071988494));
#23980=CARTESIAN_POINT('Ctrl Pts',(4.58993464005752,3.94736842105264,2.64999999999999));
#23981=CARTESIAN_POINT('Ctrl Pts',(3.87986928011505,4.14473684210529,3.87986928011504));
#23982=CARTESIAN_POINT('Ctrl Pts',(2.65,4.34210526315792,4.58993464005751));
#23983=CARTESIAN_POINT('Ctrl Pts',(1.42013071988495,4.53947368421056,5.29999999999998));
#23984=CARTESIAN_POINT('Ctrl Pts',(8.32001735975286E-29,4.73684210526315,
5.29999999999999));
#23985=CARTESIAN_POINT('Ctrl Pts',(-1.42013071988495,4.93421052631578,5.29999999999999));
#23986=CARTESIAN_POINT('Ctrl Pts',(-2.65,5.13157894736843,4.58993464005751));
#23987=CARTESIAN_POINT('Ctrl Pts',(-3.87986928011504,5.32894736842106,3.87986928011505));
#23988=CARTESIAN_POINT('Ctrl Pts',(-4.58993464005751,5.52631578947371,2.65));
#23989=CARTESIAN_POINT('Ctrl Pts',(-5.29999999999999,5.72368421052634,1.42013071988495));
#23990=CARTESIAN_POINT('Ctrl Pts',(-5.29999999999999,5.92105263157894,3.24531401774024E-16));
#23991=CARTESIAN_POINT('Ctrl Pts',(-5.29999999999999,6.11842105263156,-1.42013071988495));
#23992=CARTESIAN_POINT('Ctrl Pts',(-4.58993464005751,6.31578947368422,-2.64999999999999));
#23993=CARTESIAN_POINT('Ctrl Pts',(-3.87986928011504,6.51315789473683,-3.87986928011504));
#23994=CARTESIAN_POINT('Ctrl Pts',(-2.65,6.71052631578944,-4.58993464005751));
#23995=CARTESIAN_POINT('Ctrl Pts',(-1.42013071988495,6.90789473684211,-5.29999999999999));
#23996=CARTESIAN_POINT('Ctrl Pts',(-6.49062803548043E-16,7.10526315789473,
-5.29999999999999));
#23997=CARTESIAN_POINT('Ctrl Pts',(1.42013071988495,7.30263157894733,-5.29999999999999));
#23998=CARTESIAN_POINT('Ctrl Pts',(2.64999999999999,7.50000000000001,-4.58993464005751));
#23999=CARTESIAN_POINT('Ctrl Pts',(3.87986928011504,7.69736842105261,-3.87986928011505));
#24000=CARTESIAN_POINT('Ctrl Pts',(4.58993464005751,7.89473684210523,-2.65));
#24001=CARTESIAN_POINT('Ctrl Pts',(5.29999999999999,8.09210526315788,-1.42013071988495));
#24002=CARTESIAN_POINT('Ctrl Pts',(5.29999999999999,8.28947368421051,-9.73594205321085E-16));
#24003=CARTESIAN_POINT('Ctrl Pts',(5.29999999999999,8.48684210526316,1.42013071988495));
#24004=CARTESIAN_POINT('Ctrl Pts',(4.58993464005752,8.68421052631579,2.64999999999999));
#24005=CARTESIAN_POINT('Ctrl Pts',(3.87986928011505,8.88157894736843,3.87986928011504));
#24006=CARTESIAN_POINT('Ctrl Pts',(2.65,9.07894736842108,4.58993464005751));
#24007=CARTESIAN_POINT('Ctrl Pts',(1.42013071988495,9.27631578947371,5.29999999999999));
#24008=CARTESIAN_POINT('Ctrl Pts',(1.35585468084861E-28,9.47368421052636,
5.3));
#24009=CARTESIAN_POINT('Ctrl Pts',(-1.42013071988495,9.67105263157899,5.29999999999998));
#24010=CARTESIAN_POINT('Ctrl Pts',(-2.65,9.86842105263158,4.58993464005751));
#24011=CARTESIAN_POINT('Ctrl Pts',(-3.87986928011504,10.0657894736842,3.87986928011504));
#24012=CARTESIAN_POINT('Ctrl Pts',(-4.58993464005751,10.2631578947369,2.65));
#24013=CARTESIAN_POINT('Ctrl Pts',(-5.29999999999999,10.4605263157895,1.42013071988495));
#24014=CARTESIAN_POINT('Ctrl Pts',(-5.29999999999999,10.6578947368421,3.24531401772841E-16));
#24015=CARTESIAN_POINT('Ctrl Pts',(-5.29999999999999,10.8552631578948,-1.42013071988495));
#24016=CARTESIAN_POINT('Ctrl Pts',(-4.58993464005751,11.0526315789474,-2.64999999999999));
#24017=CARTESIAN_POINT('Ctrl Pts',(-3.87986928011504,11.25,-3.87986928011504));
#24018=CARTESIAN_POINT('Ctrl Pts',(-2.65,11.4473684210526,-4.58993464005751));
#24019=CARTESIAN_POINT('Ctrl Pts',(-1.42013071988495,11.6447368421052,-5.29999999999999));
#24020=CARTESIAN_POINT('Ctrl Pts',(-6.49062803547995E-16,11.8421052631579,
-5.29999999999999));
#24021=CARTESIAN_POINT('Ctrl Pts',(1.42013071988495,12.0394736842105,-5.29999999999999));
#24022=CARTESIAN_POINT('Ctrl Pts',(2.64999999999999,12.2368421052632,-4.58993464005751));
#24023=CARTESIAN_POINT('Ctrl Pts',(3.87986928011504,12.4342105263158,-3.87986928011505));
#24024=CARTESIAN_POINT('Ctrl Pts',(4.58993464005751,12.6315789473684,-2.65));
#24025=CARTESIAN_POINT('Ctrl Pts',(5.29999999999999,12.828947368421,-1.42013071988495));
#24026=CARTESIAN_POINT('Ctrl Pts',(5.29999999999999,13.0263157894737,-9.73594205322072E-16));
#24027=CARTESIAN_POINT('Ctrl Pts',(5.29999999999999,13.2236842105263,1.42013071988495));
#24028=CARTESIAN_POINT('Ctrl Pts',(4.58993464005752,13.4210526315789,2.64999999999999));
#24029=CARTESIAN_POINT('Ctrl Pts',(3.87986928011505,13.6184210526316,3.87986928011504));
#24030=CARTESIAN_POINT('Ctrl Pts',(2.65,13.8157894736842,4.58993464005751));
#24031=CARTESIAN_POINT('Ctrl Pts',(1.42013071988495,14.0131578947369,5.29999999999998));
#24032=CARTESIAN_POINT('Ctrl Pts',(1.84889274661175E-28,14.2105263157895,
5.3));
#24033=CARTESIAN_POINT('Ctrl Pts',(-1.42013071988495,14.4078947368421,5.29999999999999));
#24034=CARTESIAN_POINT('Ctrl Pts',(-2.65,14.6052631578947,4.58993464005751));
#24035=CARTESIAN_POINT('Ctrl Pts',(-3.87986928011504,14.8026315789474,3.87986928011504));
#24036=CARTESIAN_POINT('Ctrl Pts',(-4.58993464005751,15.,2.65));
#24037=CARTESIAN_POINT('Ctrl Pts',(-5.29999999999999,15.1973684210526,1.42013071988495));
#24038=CARTESIAN_POINT('Ctrl Pts',(-5.29999999999999,15.3947368421052,3.24531401774024E-16));
#24039=CARTESIAN_POINT('Ctrl Pts',(-5.29999999999999,15.5921052631579,-1.42013071988495));
#24040=CARTESIAN_POINT('Ctrl Pts',(-4.58993464005751,15.7894736842105,-2.64999999999999));
#24041=CARTESIAN_POINT('Ctrl Pts',(-3.87986928011504,15.9868421052631,-3.87986928011504));
#24042=CARTESIAN_POINT('Ctrl Pts',(-2.65,16.1842105263157,-4.58993464005751));
#24043=CARTESIAN_POINT('Ctrl Pts',(-1.42013071988495,16.3815789473684,-5.29999999999999));
#24044=CARTESIAN_POINT('Ctrl Pts',(-6.49062803547949E-16,16.578947368421,
-5.29999999999999));
#24045=CARTESIAN_POINT('Ctrl Pts',(1.42013071988495,16.7763157894737,-5.29999999999999));
#24046=CARTESIAN_POINT('Ctrl Pts',(2.64999999999999,16.9736842105263,-4.58993464005751));
#24047=CARTESIAN_POINT('Ctrl Pts',(3.87986928011504,17.171052631579,-3.87986928011505));
#24048=CARTESIAN_POINT('Ctrl Pts',(4.58993464005751,17.3684210526316,-2.65));
#24049=CARTESIAN_POINT('Ctrl Pts',(5.29999999999999,17.5657894736842,-1.42013071988495));
#24050=CARTESIAN_POINT('Ctrl Pts',(5.29999999999999,17.7631578947368,-9.73594205322269E-16));
#24051=CARTESIAN_POINT('Ctrl Pts',(5.29999999999999,17.9605263157895,1.42013071988494));
#24052=CARTESIAN_POINT('Ctrl Pts',(4.58993464005752,18.1578947368421,2.64999999999999));
#24053=CARTESIAN_POINT('Ctrl Pts',(3.87986928011505,18.3552631578947,3.87986928011504));
#24054=CARTESIAN_POINT('Ctrl Pts',(2.65,18.5526315789474,4.58993464005751));
#24055=CARTESIAN_POINT('Ctrl Pts',(1.42013071988495,18.75,5.29999999999998));
#24056=CARTESIAN_POINT('Ctrl Pts',(2.31111593326468E-28,18.9473684210527,
5.3));
#24057=CARTESIAN_POINT('Ctrl Pts',(-1.42013071988495,19.1447368421053,5.29999999999999));
#24058=CARTESIAN_POINT('Ctrl Pts',(-2.65,19.3421052631579,4.58993464005751));
#24059=CARTESIAN_POINT('Ctrl Pts',(-3.87986928011504,19.5394736842105,3.87986928011504));
#24060=CARTESIAN_POINT('Ctrl Pts',(-4.58993464005751,19.7368421052632,2.65));
#24061=CARTESIAN_POINT('Ctrl Pts',(-5.29999999999999,19.9342105263158,1.42013071988495));
#24062=CARTESIAN_POINT('Ctrl Pts',(-5.29999999999999,20.1315789473684,3.24531401774221E-16));
#24063=CARTESIAN_POINT('Ctrl Pts',(-5.29999999999999,20.328947368421,-1.42013071988495));
#24064=CARTESIAN_POINT('Ctrl Pts',(-4.58993464005751,20.5263157894737,-2.64999999999999));
#24065=CARTESIAN_POINT('Ctrl Pts',(-3.87986928011504,20.7236842105263,-3.87986928011504));
#24066=CARTESIAN_POINT('Ctrl Pts',(-2.65,20.921052631579,-4.58993464005751));
#24067=CARTESIAN_POINT('Ctrl Pts',(-1.42013071988495,21.1184210526315,-5.29999999999999));
#24068=CARTESIAN_POINT('Ctrl Pts',(-6.49062803547894E-16,21.3157894736842,
-5.29999999999999));
#24069=CARTESIAN_POINT('Ctrl Pts',(1.42013071988495,21.5131578947368,-5.29999999999999));
#24070=CARTESIAN_POINT('Ctrl Pts',(2.64999999999999,21.7105263157895,-4.58993464005751));
#24071=CARTESIAN_POINT('Ctrl Pts',(3.87986928011504,21.9078947368421,-3.87986928011505));
#24072=CARTESIAN_POINT('Ctrl Pts',(4.58993464005751,22.1052631578947,-2.65));
#24073=CARTESIAN_POINT('Ctrl Pts',(5.29999999999999,22.3026315789474,-1.42013071988495));
#24074=CARTESIAN_POINT('Ctrl Pts',(5.29999999999999,22.5,-9.73594205320888E-16));
#24075=CARTESIAN_POINT('Ctrl Pts',(5.29999999999999,22.6973684210527,1.42013071988495));
#24076=CARTESIAN_POINT('Ctrl Pts',(4.58993464005752,22.8947368421052,2.64999999999999));
#24077=CARTESIAN_POINT('Ctrl Pts',(3.87986928011505,23.0921052631579,3.87986928011504));
#24078=CARTESIAN_POINT('Ctrl Pts',(2.65,23.2894736842105,4.58993464005751));
#24079=CARTESIAN_POINT('Ctrl Pts',(1.42013071988495,23.4868421052631,5.29999999999999));
#24080=CARTESIAN_POINT('Ctrl Pts',(2.95822839457879E-28,23.6842105263158,
5.3));
#24081=CARTESIAN_POINT('Ctrl Pts',(-1.42013071988495,23.8815789473684,5.29999999999998));
#24082=CARTESIAN_POINT('Ctrl Pts',(-2.65,24.0789473684211,4.58993464005751));
#24083=CARTESIAN_POINT('Ctrl Pts',(-3.87986928011504,24.2763157894737,3.87986928011504));
#24084=CARTESIAN_POINT('Ctrl Pts',(-4.58993464005751,24.4736842105263,2.65));
#24085=CARTESIAN_POINT('Ctrl Pts',(-5.29999999999999,24.671052631579,1.42013071988495));
#24086=CARTESIAN_POINT('Ctrl Pts',(-5.29999999999999,24.8684210526316,3.24531401774024E-16));
#24087=CARTESIAN_POINT('Ctrl Pts',(-5.29999999999999,25.0657894736842,-1.42013071988495));
#24088=CARTESIAN_POINT('Ctrl Pts',(-4.58993464005751,25.2631578947368,-2.64999999999999));
#24089=CARTESIAN_POINT('Ctrl Pts',(-3.87986928011504,25.4605263157895,-3.87986928011504));
#24090=CARTESIAN_POINT('Ctrl Pts',(-2.65,25.6578947368421,-4.58993464005751));
#24091=CARTESIAN_POINT('Ctrl Pts',(-1.42013071988495,25.8552631578947,-5.29999999999999));
#24092=CARTESIAN_POINT('Ctrl Pts',(-6.49062803547834E-16,26.0526315789473,
-5.29999999999999));
#24093=CARTESIAN_POINT('Ctrl Pts',(1.42013071988495,26.25,-5.29999999999999));
#24094=CARTESIAN_POINT('Ctrl Pts',(2.64999999999999,26.4473684210526,-4.58993464005752));
#24095=CARTESIAN_POINT('Ctrl Pts',(3.87986928011504,26.6447368421052,-3.87986928011505));
#24096=CARTESIAN_POINT('Ctrl Pts',(4.58993464005751,26.8421052631579,-2.65));
#24097=CARTESIAN_POINT('Ctrl Pts',(5.29999999999999,27.0394736842105,-1.42013071988495));
#24098=CARTESIAN_POINT('Ctrl Pts',(5.29999999999999,27.2368421052632,-9.73594205320888E-16));
#24099=CARTESIAN_POINT('Ctrl Pts',(5.29999999999999,27.4342105263158,1.42013071988495));
#24100=CARTESIAN_POINT('Ctrl Pts',(4.58993464005752,27.6315789473685,2.64999999999999));
#24101=CARTESIAN_POINT('Ctrl Pts',(3.87986928011505,27.8289473684211,3.87986928011504));
#24102=CARTESIAN_POINT('Ctrl Pts',(2.65,28.0263157894737,4.58993464005751));
#24103=CARTESIAN_POINT('Ctrl Pts',(1.42013071988495,28.2236842105264,5.29999999999998));
#24104=CARTESIAN_POINT('Ctrl Pts',(3.42045158123173E-28,28.421052631579,
5.3));
#24105=CARTESIAN_POINT('Ctrl Pts',(-1.42013071988495,28.6184210526316,5.29999999999999));
#24106=CARTESIAN_POINT('Ctrl Pts',(-2.65,28.8157894736842,4.58993464005751));
#24107=CARTESIAN_POINT('Ctrl Pts',(-3.87986928011504,29.0131578947368,3.87986928011504));
#24108=CARTESIAN_POINT('Ctrl Pts',(-4.58993464005751,29.2105263157895,2.65));
#24109=CARTESIAN_POINT('Ctrl Pts',(-5.29999999999999,29.4078947368421,1.42013071988495));
#24110=CARTESIAN_POINT('Ctrl Pts',(-5.29999999999999,29.6052631578947,3.24531401774024E-16));
#24111=CARTESIAN_POINT('Ctrl Pts',(-5.29999999999999,29.8026315789473,-1.42013071988495));
#24112=CARTESIAN_POINT('Ctrl Pts',(-4.58993464005751,30.,-2.64999999999999));
#24113=CARTESIAN_POINT('Ctrl Pts',(-3.87986928011504,30.1973684210526,-3.87986928011504));
#24114=CARTESIAN_POINT('Ctrl Pts',(-2.65,30.3947368421053,-4.58993464005751));
#24115=CARTESIAN_POINT('Ctrl Pts',(-1.42013071988495,30.5921052631579,-5.29999999999999));
#24116=CARTESIAN_POINT('Ctrl Pts',(-6.49062803547783E-16,30.7894736842105,
-5.29999999999999));
#24117=CARTESIAN_POINT('Ctrl Pts',(1.42013071988495,30.9868421052631,-5.29999999999999));
#24118=CARTESIAN_POINT('Ctrl Pts',(2.64999999999999,31.1842105263158,-4.58993464005752));
#24119=CARTESIAN_POINT('Ctrl Pts',(3.87986928011504,31.3815789473684,-3.87986928011505));
#24120=CARTESIAN_POINT('Ctrl Pts',(4.58993464005751,31.578947368421,-2.65));
#24121=CARTESIAN_POINT('Ctrl Pts',(5.29999999999999,31.7763157894737,-1.42013071988495));
#24122=CARTESIAN_POINT('Ctrl Pts',(5.29999999999999,31.9736842105263,-9.73594205321085E-16));
#24123=CARTESIAN_POINT('Ctrl Pts',(5.29999999999999,32.1710526315789,1.42013071988495));
#24124=CARTESIAN_POINT('Ctrl Pts',(4.58993464005752,32.3684210526316,2.64999999999999));
#24125=CARTESIAN_POINT('Ctrl Pts',(3.87986928011505,32.5657894736842,3.87986928011504));
#24126=CARTESIAN_POINT('Ctrl Pts',(2.65,32.7631578947368,4.58993464005751));
#24127=CARTESIAN_POINT('Ctrl Pts',(1.42013071988495,32.9605263157895,5.29999999999999));
#24128=CARTESIAN_POINT('Ctrl Pts',(3.88267476788467E-28,33.1578947368421,
5.3));
#24129=CARTESIAN_POINT('Ctrl Pts',(-1.42013071988495,33.3552631578948,5.29999999999998));
#24130=CARTESIAN_POINT('Ctrl Pts',(-2.65,33.5526315789474,4.58993464005751));
#24131=CARTESIAN_POINT('Ctrl Pts',(-3.87986928011504,33.75,3.87986928011505));
#24132=CARTESIAN_POINT('Ctrl Pts',(-4.58993464005751,33.9473684210526,2.65));
#24133=CARTESIAN_POINT('Ctrl Pts',(-5.29999999999999,34.1447368421052,1.42013071988495));
#24134=CARTESIAN_POINT('Ctrl Pts',(-5.29999999999999,34.3421052631579,3.24531401774024E-16));
#24135=CARTESIAN_POINT('Ctrl Pts',(-5.29999999999999,34.5394736842105,-1.42013071988495));
#24136=CARTESIAN_POINT('Ctrl Pts',(-4.58993464005751,34.7368421052631,-2.65));
#24137=CARTESIAN_POINT('Ctrl Pts',(-3.87986928011504,34.9342105263158,-3.87986928011504));
#24138=CARTESIAN_POINT('Ctrl Pts',(-2.65,35.1315789473684,-4.58993464005751));
#24139=CARTESIAN_POINT('Ctrl Pts',(-1.42013071988495,35.328947368421,-5.29999999999999));
#24140=CARTESIAN_POINT('Ctrl Pts',(-6.49062803547736E-16,35.5263157894737,
-5.29999999999999));
#24141=CARTESIAN_POINT('Ctrl Pts',(1.42013071988495,35.7236842105263,-5.29999999999999));
#24142=CARTESIAN_POINT('Ctrl Pts',(2.64999999999999,35.9210526315789,-4.58993464005752));
#24143=CARTESIAN_POINT('Ctrl Pts',(3.87986928011504,36.1184210526315,-3.87986928011505));
#24144=CARTESIAN_POINT('Ctrl Pts',(4.58993464005751,36.3157894736842,-2.65));
#24145=CARTESIAN_POINT('Ctrl Pts',(5.29999999999999,36.5131578947368,-1.42013071988495));
#24146=CARTESIAN_POINT('Ctrl Pts',(5.29999999999999,36.7105263157895,-9.73594205322072E-16));
#24147=CARTESIAN_POINT('Ctrl Pts',(5.29999999999999,36.9078947368421,1.42013071988495));
#24148=CARTESIAN_POINT('Ctrl Pts',(4.58993464005752,37.1052631578948,2.64999999999999));
#24149=CARTESIAN_POINT('Ctrl Pts',(3.87986928011505,37.3026315789473,3.87986928011504));
#24150=CARTESIAN_POINT('Ctrl Pts',(2.65,37.5,4.58993464005751));
#24151=CARTESIAN_POINT('Ctrl Pts',(1.42013071988495,37.6973684210526,5.29999999999998));
#24152=CARTESIAN_POINT('Ctrl Pts',(4.42193515231309E-28,37.8947368421053,
5.29999999999999));
#24153=CARTESIAN_POINT('Ctrl Pts',(-1.42013071988495,38.0921052631579,5.29999999999999));
#24154=CARTESIAN_POINT('Ctrl Pts',(-2.65,38.2894736842105,4.58993464005752));
#24155=CARTESIAN_POINT('Ctrl Pts',(-3.87986928011504,38.4868421052632,3.87986928011504));
#24156=CARTESIAN_POINT('Ctrl Pts',(-4.58993464005751,38.6842105263158,2.65));
#24157=CARTESIAN_POINT('Ctrl Pts',(-5.29999999999999,38.8815789473684,1.42013071988495));
#24158=CARTESIAN_POINT('Ctrl Pts',(-5.29999999999999,39.078947368421,3.24531401774024E-16));
#24159=CARTESIAN_POINT('Ctrl Pts',(-5.29999999999999,39.2763157894737,-1.42013071988495));
#24160=CARTESIAN_POINT('Ctrl Pts',(-4.58993464005751,39.4736842105263,-2.64999999999999));
#24161=CARTESIAN_POINT('Ctrl Pts',(-3.87986928011504,39.6710526315789,-3.87986928011504));
#24162=CARTESIAN_POINT('Ctrl Pts',(-2.65,39.8684210526316,-4.58993464005751));
#24163=CARTESIAN_POINT('Ctrl Pts',(-1.42013071988495,40.0657894736842,-5.29999999999999));
#24164=CARTESIAN_POINT('Ctrl Pts',(-6.49062803547683E-16,40.2631578947368,
-5.29999999999999));
#24165=CARTESIAN_POINT('Ctrl Pts',(1.42013071988495,40.4605263157895,-5.29999999999999));
#24166=CARTESIAN_POINT('Ctrl Pts',(2.64999999999999,40.6578947368421,-4.58993464005752));
#24167=CARTESIAN_POINT('Ctrl Pts',(3.87986928011504,40.8552631578947,-3.87986928011505));
#24168=CARTESIAN_POINT('Ctrl Pts',(4.58993464005751,41.0526315789473,-2.65));
#24169=CARTESIAN_POINT('Ctrl Pts',(5.29999999999999,41.25,-1.42013071988495));
#24170=CARTESIAN_POINT('Ctrl Pts',(5.29999999999999,41.4473684210526,-9.73594205322072E-16));
#24171=CARTESIAN_POINT('Ctrl Pts',(5.29999999999999,41.6447368421053,1.42013071988495));
#24172=CARTESIAN_POINT('Ctrl Pts',(4.58993464005752,41.8421052631579,2.64999999999999));
#24173=CARTESIAN_POINT('Ctrl Pts',(3.87986928011505,42.0394736842106,3.87986928011504));
#24174=CARTESIAN_POINT('Ctrl Pts',(2.65,42.2368421052632,4.58993464005751));
#24175=CARTESIAN_POINT('Ctrl Pts',(1.42013071988495,42.4342105263158,5.29999999999999));
#24176=CARTESIAN_POINT('Ctrl Pts',(4.99201041585172E-28,42.6315789473684,
5.29999999999999));
#24177=CARTESIAN_POINT('Ctrl Pts',(-1.42013071988495,42.8289473684211,5.29999999999998));
#24178=CARTESIAN_POINT('Ctrl Pts',(-2.65,43.0263157894737,4.58993464005752));
#24179=CARTESIAN_POINT('Ctrl Pts',(-3.87986928011504,43.2236842105263,3.87986928011504));
#24180=CARTESIAN_POINT('Ctrl Pts',(-4.58993464005751,43.421052631579,2.65));
#24181=CARTESIAN_POINT('Ctrl Pts',(-5.29999999999999,43.6184210526316,1.42013071988495));
#24182=CARTESIAN_POINT('Ctrl Pts',(-5.29999999999999,43.8157894736842,3.24531401774024E-16));
#24183=CARTESIAN_POINT('Ctrl Pts',(-5.29999999999999,44.0131578947368,-1.42013071988495));
#24184=CARTESIAN_POINT('Ctrl Pts',(-4.58993464005751,44.2105263157895,-2.64999999999999));
#24185=CARTESIAN_POINT('Ctrl Pts',(-3.87986928011504,44.4078947368421,-3.87986928011504));
#24186=CARTESIAN_POINT('Ctrl Pts',(-2.65,44.6052631578947,-4.58993464005751));
#24187=CARTESIAN_POINT('Ctrl Pts',(-1.42013071988495,44.8026315789473,-5.29999999999999));
#24188=CARTESIAN_POINT('Ctrl Pts',(-6.49062803547635E-16,45.,-5.29999999999999));
#24189=CARTESIAN_POINT('Ctrl Pts',(1.42013071988495,45.1973684210526,-5.29999999999999));
#24190=CARTESIAN_POINT('Ctrl Pts',(2.64999999999999,45.3947368421053,-4.58993464005752));
#24191=CARTESIAN_POINT('Ctrl Pts',(3.87986928011504,45.5921052631579,-3.87986928011505));
#24192=CARTESIAN_POINT('Ctrl Pts',(4.58993464005751,45.7894736842105,-2.65));
#24193=CARTESIAN_POINT('Ctrl Pts',(5.29999999999999,45.9868421052631,-1.42013071988495));
#24194=CARTESIAN_POINT('Ctrl Pts',(5.29999999999999,46.1842105263158,-9.73594205321085E-16));
#24195=CARTESIAN_POINT('Ctrl Pts',(5.29999999999999,46.3815789473684,1.42013071988495));
#24196=CARTESIAN_POINT('Ctrl Pts',(4.58993464005752,46.5789473684211,2.64999999999999));
#24197=CARTESIAN_POINT('Ctrl Pts',(3.87986928011505,46.7763157894737,3.87986928011504));
#24198=CARTESIAN_POINT('Ctrl Pts',(2.65,46.9736842105263,4.58993464005752));
#24199=CARTESIAN_POINT('Ctrl Pts',(1.42013071988495,47.1710526315789,5.29999999999999));
#24200=CARTESIAN_POINT('Ctrl Pts',(5.54667823983524E-28,47.3684210526316,
5.29999999999999));
#24201=CARTESIAN_POINT('Ctrl Pts',(-1.42013071988495,47.5657894736842,5.29999999999998));
#24202=CARTESIAN_POINT('Ctrl Pts',(-2.65,47.7631578947368,4.58993464005752));
#24203=CARTESIAN_POINT('Ctrl Pts',(-3.87986928011504,47.9605263157895,3.87986928011504));
#24204=CARTESIAN_POINT('Ctrl Pts',(-4.58993464005751,48.1578947368421,2.65));
#24205=CARTESIAN_POINT('Ctrl Pts',(-5.29999999999999,48.3552631578947,1.42013071988495));
#24206=CARTESIAN_POINT('Ctrl Pts',(-5.29999999999999,48.5526315789474,3.24531401773827E-16));
#24207=CARTESIAN_POINT('Ctrl Pts',(-5.29999999999999,48.75,-1.42013071988495));
#24208=CARTESIAN_POINT('Ctrl Pts',(-4.58993464005751,48.9473684210526,-2.64999999999999));
#24209=CARTESIAN_POINT('Ctrl Pts',(-3.87986928011504,49.1447368421053,-3.87986928011504));
#24210=CARTESIAN_POINT('Ctrl Pts',(-2.65,49.3421052631579,-4.58993464005751));
#24211=CARTESIAN_POINT('Ctrl Pts',(-1.42013071988495,49.5394736842105,-5.29999999999999));
#24212=CARTESIAN_POINT('Ctrl Pts',(-6.49062803547579E-16,49.7368421052631,
-5.29999999999999));
#24213=CARTESIAN_POINT('Ctrl Pts',(1.42013071988495,49.9342105263158,-5.29999999999999));
#24214=CARTESIAN_POINT('Ctrl Pts',(2.64999999999999,50.1315789473684,-4.58993464005752));
#24215=CARTESIAN_POINT('Ctrl Pts',(3.87986928011504,50.328947368421,-3.87986928011505));
#24216=CARTESIAN_POINT('Ctrl Pts',(4.58993464005751,50.5263157894737,-2.65));
#24217=CARTESIAN_POINT('Ctrl Pts',(5.29999999999999,50.7236842105263,-1.42013071988495));
#24218=CARTESIAN_POINT('Ctrl Pts',(5.29999999999999,50.9210526315789,-9.73594205321085E-16));
#24219=CARTESIAN_POINT('Ctrl Pts',(5.29999999999999,51.1184210526316,1.42013071988495));
#24220=CARTESIAN_POINT('Ctrl Pts',(4.58993464005752,51.3157894736842,2.64999999999999));
#24221=CARTESIAN_POINT('Ctrl Pts',(3.87986928011505,51.5131578947368,3.87986928011504));
#24222=CARTESIAN_POINT('Ctrl Pts',(2.65,51.7105263157895,4.58993464005752));
#24223=CARTESIAN_POINT('Ctrl Pts',(1.42013071988495,51.9078947368421,5.29999999999998));
#24224=CARTESIAN_POINT('Ctrl Pts',(6.00890142648818E-28,52.1052631578948,
5.29999999999999));
#24225=CARTESIAN_POINT('Ctrl Pts',(-1.42013071988495,52.3026315789474,5.29999999999999));
#24226=CARTESIAN_POINT('Ctrl Pts',(-2.65,52.5,4.58993464005752));
#24227=CARTESIAN_POINT('Ctrl Pts',(-3.87986928011504,52.6973684210526,3.87986928011504));
#24228=CARTESIAN_POINT('Ctrl Pts',(-4.58993464005751,52.8947368421053,2.65));
#24229=CARTESIAN_POINT('Ctrl Pts',(-5.29999999999999,53.0921052631579,1.42013071988495));
#24230=CARTESIAN_POINT('Ctrl Pts',(-5.29999999999999,53.2894736842105,3.245314017757E-16));
#24231=CARTESIAN_POINT('Ctrl Pts',(-5.29999999999999,53.4868421052631,-1.42013071988495));
#24232=CARTESIAN_POINT('Ctrl Pts',(-4.58993464005751,53.6842105263158,-2.64999999999999));
#24233=CARTESIAN_POINT('Ctrl Pts',(-3.87986928011504,53.8815789473684,-3.87986928011504));
#24234=CARTESIAN_POINT('Ctrl Pts',(-2.65,54.0789473684211,-4.58993464005751));
#24235=CARTESIAN_POINT('Ctrl Pts',(-1.42013071988495,54.2763157894737,-5.29999999999999));
#24236=CARTESIAN_POINT('Ctrl Pts',(-6.4906280354753E-16,54.4736842105263,
-5.29999999999999));
#24237=CARTESIAN_POINT('Ctrl Pts',(1.42013071988495,54.6710526315789,-5.29999999999999));
#24238=CARTESIAN_POINT('Ctrl Pts',(2.64999999999999,54.8684210526316,-4.58993464005752));
#24239=CARTESIAN_POINT('Ctrl Pts',(3.87986928011504,55.0657894736842,-3.87986928011505));
#24240=CARTESIAN_POINT('Ctrl Pts',(4.58993464005751,55.2631578947368,-2.65));
#24241=CARTESIAN_POINT('Ctrl Pts',(5.29999999999999,55.4605263157895,-1.42013071988495));
#24242=CARTESIAN_POINT('Ctrl Pts',(5.29999999999999,55.6578947368421,-9.73594205321578E-16));
#24243=CARTESIAN_POINT('Ctrl Pts',(5.29999999999999,55.8552631578947,1.42013071988495));
#24244=CARTESIAN_POINT('Ctrl Pts',(4.58993464005752,56.0526315789474,2.64999999999999));
#24245=CARTESIAN_POINT('Ctrl Pts',(3.87986928011505,56.25,3.87986928011504));
#24246=CARTESIAN_POINT('Ctrl Pts',(2.65,56.4473684210526,4.58993464005752));
#24247=CARTESIAN_POINT('Ctrl Pts',(1.42013071988495,56.6447368421052,5.29999999999999));
#24248=CARTESIAN_POINT('Ctrl Pts',(6.5635692504717E-28,56.8421052631579,
5.29999999999999));
#24249=CARTESIAN_POINT('Ctrl Pts',(-1.42013071988495,57.0394736842105,5.29999999999998));
#24250=CARTESIAN_POINT('Ctrl Pts',(-2.65,57.2368421052632,4.58993464005752));
#24251=CARTESIAN_POINT('Ctrl Pts',(-3.87986928011504,57.4342105263158,3.87986928011504));
#24252=CARTESIAN_POINT('Ctrl Pts',(-4.58993464005751,57.6315789473684,2.65));
#24253=CARTESIAN_POINT('Ctrl Pts',(-5.29999999999999,57.8289473684211,1.42013071988495));
#24254=CARTESIAN_POINT('Ctrl Pts',(-5.29999999999999,58.0263157894737,3.24531401775207E-16));
#24255=CARTESIAN_POINT('Ctrl Pts',(-5.29999999999999,58.2236842105263,-1.42013071988495));
#24256=CARTESIAN_POINT('Ctrl Pts',(-4.58993464005751,58.4210526315789,-2.64999999999999));
#24257=CARTESIAN_POINT('Ctrl Pts',(-3.87986928011504,58.6184210526315,-3.87986928011504));
#24258=CARTESIAN_POINT('Ctrl Pts',(-2.65,58.8157894736842,-4.58993464005751));
#24259=CARTESIAN_POINT('Ctrl Pts',(-1.42013071988495,59.0131578947368,-5.29999999999999));
#24260=CARTESIAN_POINT('Ctrl Pts',(-6.49062803547473E-16,59.2105263157894,
-5.29999999999999));
#24261=CARTESIAN_POINT('Ctrl Pts',(1.42013071988495,59.4078947368421,-5.29999999999999));
#24262=CARTESIAN_POINT('Ctrl Pts',(2.64999999999999,59.6052631578947,-4.58993464005752));
#24263=CARTESIAN_POINT('Ctrl Pts',(3.87986928011504,59.8026315789473,-3.87986928011505));
#24264=CARTESIAN_POINT('Ctrl Pts',(4.58993464005751,60.,-2.65));
#24265=CARTESIAN_POINT('Ctrl Pts',(5.29999999999999,60.1973684210526,-1.42013071988495));
#24266=CARTESIAN_POINT('Ctrl Pts',(5.29999999999999,60.3947368421052,-9.73594205321184E-16));
#24267=CARTESIAN_POINT('Ctrl Pts',(5.29999999999999,60.5921052631579,1.42013071988495));
#24268=CARTESIAN_POINT('Ctrl Pts',(4.58993464005752,60.7894736842105,2.64999999999999));
#24269=CARTESIAN_POINT('Ctrl Pts',(3.87986928011505,60.9868421052632,3.87986928011504));
#24270=CARTESIAN_POINT('Ctrl Pts',(2.65,61.1842105263158,4.58993464005752));
#24271=CARTESIAN_POINT('Ctrl Pts',(1.42013071988495,61.3815789473684,5.29999999999998));
#24272=CARTESIAN_POINT('Ctrl Pts',(7.02579243712464E-28,61.5789473684211,
5.29999999999999));
#24273=CARTESIAN_POINT('Ctrl Pts',(-1.42013071988495,61.7763157894737,5.29999999999999));
#24274=CARTESIAN_POINT('Ctrl Pts',(-2.65,61.9736842105264,4.58993464005752));
#24275=CARTESIAN_POINT('Ctrl Pts',(-3.87986928011504,62.171052631579,3.87986928011505));
#24276=CARTESIAN_POINT('Ctrl Pts',(-4.58993464005751,62.3684210526316,2.65));
#24277=CARTESIAN_POINT('Ctrl Pts',(-5.29999999999999,62.5657894736842,1.42013071988495));
#24278=CARTESIAN_POINT('Ctrl Pts',(-5.29999999999999,62.7631578947368,3.24531401775109E-16));
#24279=CARTESIAN_POINT('Ctrl Pts',(-5.29999999999999,62.9605263157895,-1.42013071988495));
#24280=CARTESIAN_POINT('Ctrl Pts',(-4.58993464005751,63.1578947368421,-2.64999999999999));
#24281=CARTESIAN_POINT('Ctrl Pts',(-3.87986928011504,63.3552631578947,-3.87986928011504));
#24282=CARTESIAN_POINT('Ctrl Pts',(-2.65,63.5526315789474,-4.58993464005751));
#24283=CARTESIAN_POINT('Ctrl Pts',(-1.42013071988495,63.75,-5.29999999999999));
#24284=CARTESIAN_POINT('Ctrl Pts',(-6.49062803547422E-16,63.9473684210526,
-5.29999999999999));
#24285=CARTESIAN_POINT('Ctrl Pts',(1.42013071988495,64.1447368421053,-5.29999999999999));
#24286=CARTESIAN_POINT('Ctrl Pts',(2.64999999999999,64.3421052631579,-4.58993464005752));
#24287=CARTESIAN_POINT('Ctrl Pts',(3.87986928011504,64.5394736842105,-3.87986928011505));
#24288=CARTESIAN_POINT('Ctrl Pts',(4.58993464005751,64.7368421052632,-2.65));
#24289=CARTESIAN_POINT('Ctrl Pts',(5.29999999999999,64.9342105263157,-1.42013071988495));
#24290=CARTESIAN_POINT('Ctrl Pts',(5.29999999999999,65.1315789473684,-9.73594205320987E-16));
#24291=CARTESIAN_POINT('Ctrl Pts',(5.29999999999999,65.328947368421,1.42013071988495));
#24292=CARTESIAN_POINT('Ctrl Pts',(4.58993464005752,65.5263157894737,2.64999999999999));
#24293=CARTESIAN_POINT('Ctrl Pts',(3.87986928011505,65.7236842105264,3.87986928011504));
#24294=CARTESIAN_POINT('Ctrl Pts',(2.65,65.9210526315789,4.58993464005752));
#24295=CARTESIAN_POINT('Ctrl Pts',(1.42013071988495,66.1184210526315,5.29999999999999));
#24296=CARTESIAN_POINT('Ctrl Pts',(7.48801562377757E-28,66.3157894736842,
5.29999999999999));
#24297=CARTESIAN_POINT('Ctrl Pts',(-1.42013071988495,66.5131578947368,5.29999999999998));
#24298=CARTESIAN_POINT('Ctrl Pts',(-2.65,66.7105263157894,4.58993464005752));
#24299=CARTESIAN_POINT('Ctrl Pts',(-3.87986928011504,66.9078947368421,3.87986928011504));
#24300=CARTESIAN_POINT('Ctrl Pts',(-4.58993464005751,67.1052631578947,2.65));
#24301=CARTESIAN_POINT('Ctrl Pts',(-5.29999999999999,67.3026315789474,1.42013071988495));
#24302=CARTESIAN_POINT('Ctrl Pts',(-5.29999999999999,67.5,3.24531401774714E-16));
#24303=CARTESIAN_POINT('Ctrl Pts',(-5.29999999999999,67.6973684210526,-1.42013071988495));
#24304=CARTESIAN_POINT('Ctrl Pts',(-4.58993464005751,67.8947368421052,-2.64999999999999));
#24305=CARTESIAN_POINT('Ctrl Pts',(-3.87986928011504,68.0921052631578,-3.87986928011504));
#24306=CARTESIAN_POINT('Ctrl Pts',(-2.65,68.2894736842105,-4.58993464005751));
#24307=CARTESIAN_POINT('Ctrl Pts',(-1.42013071988495,68.4868421052632,-5.29999999999999));
#24308=CARTESIAN_POINT('Ctrl Pts',(-6.49062803547376E-16,68.6842105263158,
-5.29999999999999));
#24309=CARTESIAN_POINT('Ctrl Pts',(1.42013071988495,68.8815789473684,-5.29999999999999));
#24310=CARTESIAN_POINT('Ctrl Pts',(2.64999999999999,69.078947368421,-4.58993464005752));
#24311=CARTESIAN_POINT('Ctrl Pts',(3.87986928011504,69.2763157894736,-3.87986928011505));
#24312=CARTESIAN_POINT('Ctrl Pts',(4.58993464005751,69.4736842105263,-2.65));
#24313=CARTESIAN_POINT('Ctrl Pts',(5.29999999999999,69.6710526315789,-1.42013071988495));
#24314=CARTESIAN_POINT('Ctrl Pts',(5.29999999999999,69.8684210526316,-9.73594205320888E-16));
#24315=CARTESIAN_POINT('Ctrl Pts',(5.29999999999999,70.0657894736842,1.42013071988495));
#24316=CARTESIAN_POINT('Ctrl Pts',(4.58993464005752,70.2631578947369,2.64999999999999));
#24317=CARTESIAN_POINT('Ctrl Pts',(3.87986928011505,70.4605263157895,3.87986928011504));
#24318=CARTESIAN_POINT('Ctrl Pts',(2.65,70.6578947368421,4.58993464005752));
#24319=CARTESIAN_POINT('Ctrl Pts',(1.42013071988495,70.8552631578947,5.29999999999998));
#24320=CARTESIAN_POINT('Ctrl Pts',(7.96564624998561E-28,71.0526315789473,
5.29999999999999));
#24321=CARTESIAN_POINT('Ctrl Pts',(-1.42013071988495,71.2499999999999,5.29999999999999));
#24322=CARTESIAN_POINT('Ctrl Pts',(-2.65,71.4473684210526,4.58993464005751));
#24323=CARTESIAN_POINT('Ctrl Pts',(-3.87986928011504,71.6447368421053,3.87986928011504));
#24324=CARTESIAN_POINT('Ctrl Pts',(-4.58993464005751,71.8421052631579,2.65));
#24325=CARTESIAN_POINT('Ctrl Pts',(-5.29999999999999,72.0394736842105,1.42013071988495));
#24326=CARTESIAN_POINT('Ctrl Pts',(-5.29999999999999,72.2368421052632,3.24531401775306E-16));
#24327=CARTESIAN_POINT('Ctrl Pts',(-5.29999999999999,72.4342105263157,-1.42013071988495));
#24328=CARTESIAN_POINT('Ctrl Pts',(-4.58993464005751,72.6315789473684,-2.64999999999999));
#24329=CARTESIAN_POINT('Ctrl Pts',(-3.87986928011504,72.828947368421,-3.87986928011504));
#24330=CARTESIAN_POINT('Ctrl Pts',(-2.65,73.0263157894737,-4.58993464005751));
#24331=CARTESIAN_POINT('Ctrl Pts',(-1.42013071988495,73.2236842105263,-5.29999999999999));
#24332=CARTESIAN_POINT('Ctrl Pts',(-6.4906280354732E-16,73.421052631579,
-5.29999999999999));
#24333=CARTESIAN_POINT('Ctrl Pts',(1.42013071988495,73.6184210526315,-5.29999999999999));
#24334=CARTESIAN_POINT('Ctrl Pts',(2.64999999999999,73.8157894736842,-4.58993464005751));
#24335=CARTESIAN_POINT('Ctrl Pts',(3.87986928011504,74.0131578947368,-3.87986928011505));
#24336=CARTESIAN_POINT('Ctrl Pts',(4.58993464005751,74.2105263157895,-2.65));
#24337=CARTESIAN_POINT('Ctrl Pts',(5.29999999999999,74.4078947368421,-1.42013071988495));
#24338=CARTESIAN_POINT('Ctrl Pts',(5.29999999999999,74.6052631578947,-9.73594205321085E-16));
#24339=CARTESIAN_POINT('Ctrl Pts',(5.29999999999999,74.8026315789473,1.42013071988495));
#24340=CARTESIAN_POINT('Ctrl Pts',(4.58993464005752,75.,2.64999999999999));
#24341=CARTESIAN_POINT('Ctrl Pts',(3.87986928011505,75.1973684210526,3.87986928011504));
#24342=CARTESIAN_POINT('Ctrl Pts',(2.65,75.3947368421052,4.58993464005751));
#24343=CARTESIAN_POINT('Ctrl Pts',(1.42013071988495,75.5921052631578,5.29999999999998));
#24344=CARTESIAN_POINT('Ctrl Pts',(8.68979590907521E-28,75.7894736842105,
5.29999999999999));
#24345=CARTESIAN_POINT('Ctrl Pts',(-1.42013071988495,75.9868421052631,5.29999999999999));
#24346=CARTESIAN_POINT('Ctrl Pts',(-2.65,76.1842105263158,4.58993464005751));
#24347=CARTESIAN_POINT('Ctrl Pts',(-3.87986928011504,76.3815789473684,3.87986928011504));
#24348=CARTESIAN_POINT('Ctrl Pts',(-4.58993464005751,76.5789473684211,2.65));
#24349=CARTESIAN_POINT('Ctrl Pts',(-5.29999999999999,76.7763157894737,1.42013071988495));
#24350=CARTESIAN_POINT('Ctrl Pts',(-5.29999999999999,76.9736842105263,3.24531401774615E-16));
#24351=CARTESIAN_POINT('Ctrl Pts',(-5.29999999999999,77.1710526315789,-1.42013071988495));
#24352=CARTESIAN_POINT('Ctrl Pts',(-4.58993464005751,77.3684210526315,-2.64999999999999));
#24353=CARTESIAN_POINT('Ctrl Pts',(-3.87986928011504,77.5657894736842,-3.87986928011504));
#24354=CARTESIAN_POINT('Ctrl Pts',(-2.65,77.7631578947368,-4.58993464005751));
#24355=CARTESIAN_POINT('Ctrl Pts',(-1.42013071988495,77.9605263157895,-5.29999999999999));
#24356=CARTESIAN_POINT('Ctrl Pts',(-6.49062803547265E-16,78.1578947368421,
-5.29999999999999));
#24357=CARTESIAN_POINT('Ctrl Pts',(1.42013071988495,78.3552631578948,-5.29999999999999));
#24358=CARTESIAN_POINT('Ctrl Pts',(2.64999999999999,78.5526315789474,-4.58993464005751));
#24359=CARTESIAN_POINT('Ctrl Pts',(3.87986928011504,78.7499999999999,-3.87986928011505));
#24360=CARTESIAN_POINT('Ctrl Pts',(4.58993464005751,78.9473684210526,-2.65));
#24361=CARTESIAN_POINT('Ctrl Pts',(5.29999999999999,79.1447368421052,-1.42013071988495));
#24362=CARTESIAN_POINT('Ctrl Pts',(5.29999999999999,79.3421052631579,-9.73594205320987E-16));
#24363=CARTESIAN_POINT('Ctrl Pts',(5.29999999999999,79.5394736842105,1.42013071988495));
#24364=CARTESIAN_POINT('Ctrl Pts',(4.58993464005752,79.7368421052632,2.64999999999999));
#24365=CARTESIAN_POINT('Ctrl Pts',(3.87986928011505,79.9342105263158,3.87986928011504));
#24366=CARTESIAN_POINT('Ctrl Pts',(2.65,80.1315789473684,4.58993464005751));
#24367=CARTESIAN_POINT('Ctrl Pts',(1.42013071988495,80.328947368421,5.29999999999999));
#24368=CARTESIAN_POINT('Ctrl Pts',(9.15201909572814E-28,80.5263157894736,
5.3));
#24369=CARTESIAN_POINT('Ctrl Pts',(-1.42013071988495,80.7236842105263,5.29999999999998));
#24370=CARTESIAN_POINT('Ctrl Pts',(-2.65,80.9210526315789,4.58993464005751));
#24371=CARTESIAN_POINT('Ctrl Pts',(-3.87986928011504,81.1184210526315,3.87986928011504));
#24372=CARTESIAN_POINT('Ctrl Pts',(-4.58993464005751,81.3157894736842,2.64999999999999));
#24373=CARTESIAN_POINT('Ctrl Pts',(-5.29999999999999,81.5131578947368,1.42013071988495));
#24374=CARTESIAN_POINT('Ctrl Pts',(-5.29999999999999,81.7105263157895,3.24531401775207E-16));
#24375=CARTESIAN_POINT('Ctrl Pts',(-5.29999999999999,81.9078947368421,-1.42013071988495));
#24376=CARTESIAN_POINT('Ctrl Pts',(-4.58993464005751,82.1052631578947,-2.64999999999999));
#24377=CARTESIAN_POINT('Ctrl Pts',(-3.87986928011504,82.3026315789473,-3.87986928011504));
#24378=CARTESIAN_POINT('Ctrl Pts',(-2.65,82.5,-4.58993464005751));
#24379=CARTESIAN_POINT('Ctrl Pts',(-1.42013071988495,82.6973684210527,-5.29999999999999));
#24380=CARTESIAN_POINT('Ctrl Pts',(-6.49062803547219E-16,82.8947368421053,
-5.29999999999999));
#24381=CARTESIAN_POINT('Ctrl Pts',(1.42013071988495,83.0921052631579,-5.29999999999999));
#24382=CARTESIAN_POINT('Ctrl Pts',(2.64999999999999,83.2894736842105,-4.58993464005751));
#24383=CARTESIAN_POINT('Ctrl Pts',(3.87986928011504,83.4868421052631,-3.87986928011505));
#24384=CARTESIAN_POINT('Ctrl Pts',(4.58993464005751,83.6842105263158,-2.65));
#24385=CARTESIAN_POINT('Ctrl Pts',(5.29999999999999,83.8815789473684,-1.42013071988495));
#24386=CARTESIAN_POINT('Ctrl Pts',(5.29999999999999,84.078947368421,-9.73594205321184E-16));
#24387=CARTESIAN_POINT('Ctrl Pts',(5.29999999999999,84.2763157894736,1.42013071988495));
#24388=CARTESIAN_POINT('Ctrl Pts',(4.58993464005752,84.4736842105263,2.64999999999999));
#24389=CARTESIAN_POINT('Ctrl Pts',(3.87986928011505,84.6710526315789,3.87986928011504));
#24390=CARTESIAN_POINT('Ctrl Pts',(2.65,84.8684210526316,4.58993464005751));
#24391=CARTESIAN_POINT('Ctrl Pts',(1.42013071988495,85.0657894736842,5.29999999999998));
#24392=CARTESIAN_POINT('Ctrl Pts',(9.61424228238108E-28,85.2631578947368,
5.3));
#24393=CARTESIAN_POINT('Ctrl Pts',(-1.42013071988495,85.4605263157894,5.29999999999999));
#24394=CARTESIAN_POINT('Ctrl Pts',(-2.65,85.6578947368421,4.58993464005751));
#24395=CARTESIAN_POINT('Ctrl Pts',(-3.87986928011504,85.8552631578947,3.87986928011504));
#24396=CARTESIAN_POINT('Ctrl Pts',(-4.58993464005751,86.0526315789474,2.65));
#24397=CARTESIAN_POINT('Ctrl Pts',(-5.29999999999999,86.25,1.42013071988495));
#24398=CARTESIAN_POINT('Ctrl Pts',(-5.29999999999999,86.4473684210526,3.24531401775207E-16));
#24399=CARTESIAN_POINT('Ctrl Pts',(-5.29999999999999,86.6447368421052,-1.42013071988495));
#24400=CARTESIAN_POINT('Ctrl Pts',(-4.58993464005751,86.8421052631579,-2.64999999999999));
#24401=CARTESIAN_POINT('Ctrl Pts',(-3.87986928011504,87.0394736842105,-3.87986928011504));
#24402=CARTESIAN_POINT('Ctrl Pts',(-2.65,87.2368421052631,-4.58993464005751));
#24403=CARTESIAN_POINT('Ctrl Pts',(-1.42013071988495,87.4342105263158,-5.29999999999999));
#24404=CARTESIAN_POINT('Ctrl Pts',(-6.49062803547173E-16,87.6315789473684,
-5.29999999999999));
#24405=CARTESIAN_POINT('Ctrl Pts',(1.42013071988495,87.828947368421,-5.29999999999999));
#24406=CARTESIAN_POINT('Ctrl Pts',(2.64999999999999,88.0263157894737,-4.58993464005751));
#24407=CARTESIAN_POINT('Ctrl Pts',(3.87986928011504,88.2236842105263,-3.87986928011505));
#24408=CARTESIAN_POINT('Ctrl Pts',(4.58993464005751,88.4210526315789,-2.65));
#24409=CARTESIAN_POINT('Ctrl Pts',(5.29999999999999,88.6184210526316,-1.42013071988495));
#24410=CARTESIAN_POINT('Ctrl Pts',(5.29999999999999,88.8157894736842,-9.73594205321085E-16));
#24411=CARTESIAN_POINT('Ctrl Pts',(5.29999999999999,89.0131578947368,1.42013071988495));
#24412=CARTESIAN_POINT('Ctrl Pts',(4.58993464005752,89.2105263157895,2.64999999999999));
#24413=CARTESIAN_POINT('Ctrl Pts',(3.87986928011505,89.4078947368421,3.87986928011504));
#24414=CARTESIAN_POINT('Ctrl Pts',(2.65,89.6052631578947,4.58993464005751));
#24415=CARTESIAN_POINT('Ctrl Pts',(1.42013071988495,89.8026315789473,5.29999999999999));
#24416=CARTESIAN_POINT('Ctrl Pts',(1.01689101063646E-27,89.9999999999999,
5.3));
#24417=CARTESIAN_POINT('Ctrl Pts',(6.93334779979405E-29,4.00000000000002,
5.29999999999999));
#24418=CARTESIAN_POINT('Ctrl Pts',(-1.42013071988495,4.19736842105264,5.29999999999999));
#24419=CARTESIAN_POINT('Ctrl Pts',(-2.65,4.3947368421053,4.58993464005751));
#24420=CARTESIAN_POINT('Ctrl Pts',(-3.87986928011504,4.5921052631579,3.87986928011504));
#24421=CARTESIAN_POINT('Ctrl Pts',(-4.58993464005752,4.78947368421054,2.65));
#24422=CARTESIAN_POINT('Ctrl Pts',(-5.29999999999999,4.98684210526316,1.42013071988495));
#24423=CARTESIAN_POINT('Ctrl Pts',(-5.29999999999999,5.18421052631578,3.24531401773092E-16));
#24424=CARTESIAN_POINT('Ctrl Pts',(-5.29999999999999,5.38157894736842,-1.42013071988495));
#24425=CARTESIAN_POINT('Ctrl Pts',(-4.58993464005752,5.57894736842106,-2.65));
#24426=CARTESIAN_POINT('Ctrl Pts',(-3.87986928011504,5.77631578947368,-3.87986928011504));
#24427=CARTESIAN_POINT('Ctrl Pts',(-2.65,5.9736842105263,-4.58993464005752));
#24428=CARTESIAN_POINT('Ctrl Pts',(-1.42013071988495,6.17105263157895,-5.29999999999999));
#24429=CARTESIAN_POINT('Ctrl Pts',(-6.49062803548048E-16,6.36842105263158,
-5.29999999999999));
#24430=CARTESIAN_POINT('Ctrl Pts',(1.42013071988495,6.56578947368421,-5.29999999999999));
#24431=CARTESIAN_POINT('Ctrl Pts',(2.65,6.76315789473682,-4.58993464005752));
#24432=CARTESIAN_POINT('Ctrl Pts',(3.87986928011504,6.96052631578947,-3.87986928011504));
#24433=CARTESIAN_POINT('Ctrl Pts',(4.58993464005752,7.1578947368421,-2.65));
#24434=CARTESIAN_POINT('Ctrl Pts',(5.29999999999999,7.35526315789473,-1.42013071988495));
#24435=CARTESIAN_POINT('Ctrl Pts',(5.29999999999999,7.55263157894738,-9.73594205321327E-16));
#24436=CARTESIAN_POINT('Ctrl Pts',(5.29999999999999,7.75,1.42013071988495));
#24437=CARTESIAN_POINT('Ctrl Pts',(4.58993464005752,7.94736842105266,2.64999999999999));
#24438=CARTESIAN_POINT('Ctrl Pts',(3.87986928011504,8.14473684210526,3.87986928011504));
#24439=CARTESIAN_POINT('Ctrl Pts',(2.65,8.3421052631579,4.58993464005751));
#24440=CARTESIAN_POINT('Ctrl Pts',(1.42013071988495,8.53947368421056,5.29999999999999));
#24441=CARTESIAN_POINT('Ctrl Pts',(1.24800260396293E-28,8.73684210526318,
5.29999999999999));
#24442=CARTESIAN_POINT('Ctrl Pts',(-1.42013071988495,8.93421052631582,5.29999999999999));
#24443=CARTESIAN_POINT('Ctrl Pts',(-2.65,9.13157894736842,4.58993464005752));
#24444=CARTESIAN_POINT('Ctrl Pts',(-3.87986928011504,9.32894736842109,3.87986928011504));
#24445=CARTESIAN_POINT('Ctrl Pts',(-4.58993464005752,9.5263157894737,2.65));
#24446=CARTESIAN_POINT('Ctrl Pts',(-5.29999999999999,9.7236842105263,1.42013071988495));
#24447=CARTESIAN_POINT('Ctrl Pts',(-5.29999999999999,9.92105263157894,3.24531401773092E-16));
#24448=CARTESIAN_POINT('Ctrl Pts',(-5.29999999999999,10.1184210526316,-1.42013071988495));
#24449=CARTESIAN_POINT('Ctrl Pts',(-4.58993464005752,10.3157894736842,-2.65));
#24450=CARTESIAN_POINT('Ctrl Pts',(-3.87986928011504,10.5131578947368,-3.87986928011504));
#24451=CARTESIAN_POINT('Ctrl Pts',(-2.65,10.7105263157895,-4.58993464005752));
#24452=CARTESIAN_POINT('Ctrl Pts',(-1.42013071988495,10.9078947368421,-5.29999999999999));
#24453=CARTESIAN_POINT('Ctrl Pts',(-6.49062803548001E-16,11.1052631578947,
-5.3));
#24454=CARTESIAN_POINT('Ctrl Pts',(1.42013071988495,11.3026315789474,-5.29999999999999));
#24455=CARTESIAN_POINT('Ctrl Pts',(2.65,11.5,-4.58993464005752));
#24456=CARTESIAN_POINT('Ctrl Pts',(3.87986928011504,11.6973684210526,-3.87986928011504));
#24457=CARTESIAN_POINT('Ctrl Pts',(4.58993464005752,11.8947368421053,-2.65));
#24458=CARTESIAN_POINT('Ctrl Pts',(5.29999999999999,12.0921052631579,-1.42013071988495));
#24459=CARTESIAN_POINT('Ctrl Pts',(5.29999999999999,12.2894736842105,-9.73594205321327E-16));
#24460=CARTESIAN_POINT('Ctrl Pts',(5.29999999999999,12.4868421052632,1.42013071988495));
#24461=CARTESIAN_POINT('Ctrl Pts',(4.58993464005752,12.6842105263158,2.64999999999999));
#24462=CARTESIAN_POINT('Ctrl Pts',(3.87986928011504,12.8815789473684,3.87986928011504));
#24463=CARTESIAN_POINT('Ctrl Pts',(2.65,13.0789473684211,4.58993464005752));
#24464=CARTESIAN_POINT('Ctrl Pts',(1.42013071988495,13.2763157894737,5.29999999999999));
#24465=CARTESIAN_POINT('Ctrl Pts',(1.80267042794645E-28,13.4736842105263,
5.29999999999999));
#24466=CARTESIAN_POINT('Ctrl Pts',(-1.42013071988495,13.671052631579,5.29999999999999));
#24467=CARTESIAN_POINT('Ctrl Pts',(-2.65,13.8684210526316,4.58993464005752));
#24468=CARTESIAN_POINT('Ctrl Pts',(-3.87986928011504,14.0657894736842,3.87986928011504));
#24469=CARTESIAN_POINT('Ctrl Pts',(-4.58993464005752,14.2631578947369,2.65));
#24470=CARTESIAN_POINT('Ctrl Pts',(-5.29999999999999,14.4605263157895,1.42013071988495));
#24471=CARTESIAN_POINT('Ctrl Pts',(-5.29999999999999,14.6578947368421,3.2453140177324E-16));
#24472=CARTESIAN_POINT('Ctrl Pts',(-5.29999999999999,14.8552631578947,-1.42013071988495));
#24473=CARTESIAN_POINT('Ctrl Pts',(-4.58993464005752,15.0526315789473,-2.64999999999999));
#24474=CARTESIAN_POINT('Ctrl Pts',(-3.87986928011504,15.25,-3.87986928011504));
#24475=CARTESIAN_POINT('Ctrl Pts',(-2.65,15.4473684210526,-4.58993464005752));
#24476=CARTESIAN_POINT('Ctrl Pts',(-1.42013071988495,15.6447368421052,-5.29999999999999));
#24477=CARTESIAN_POINT('Ctrl Pts',(-6.49062803547951E-16,15.8421052631579,
-5.29999999999999));
#24478=CARTESIAN_POINT('Ctrl Pts',(1.42013071988495,16.0394736842105,-5.29999999999999));
#24479=CARTESIAN_POINT('Ctrl Pts',(2.65,16.2368421052631,-4.58993464005752));
#24480=CARTESIAN_POINT('Ctrl Pts',(3.87986928011504,16.4342105263158,-3.87986928011504));
#24481=CARTESIAN_POINT('Ctrl Pts',(4.58993464005752,16.6315789473684,-2.65));
#24482=CARTESIAN_POINT('Ctrl Pts',(5.29999999999999,16.8289473684211,-1.42013071988495));
#24483=CARTESIAN_POINT('Ctrl Pts',(5.29999999999999,17.0263157894737,-9.73594205321327E-16));
#24484=CARTESIAN_POINT('Ctrl Pts',(5.29999999999999,17.2236842105263,1.42013071988494));
#24485=CARTESIAN_POINT('Ctrl Pts',(4.58993464005752,17.4210526315789,2.64999999999999));
#24486=CARTESIAN_POINT('Ctrl Pts',(3.87986928011504,17.6184210526316,3.87986928011504));
#24487=CARTESIAN_POINT('Ctrl Pts',(2.65,17.8157894736842,4.58993464005751));
#24488=CARTESIAN_POINT('Ctrl Pts',(1.42013071988495,18.0131578947369,5.29999999999999));
#24489=CARTESIAN_POINT('Ctrl Pts',(2.28800477393204E-28,18.2105263157895,
5.29999999999999));
#24490=CARTESIAN_POINT('Ctrl Pts',(-1.42013071988495,18.4078947368421,5.29999999999999));
#24491=CARTESIAN_POINT('Ctrl Pts',(-2.65,18.6052631578947,4.58993464005751));
#24492=CARTESIAN_POINT('Ctrl Pts',(-3.87986928011504,18.8026315789474,3.87986928011505));
#24493=CARTESIAN_POINT('Ctrl Pts',(-4.58993464005752,19.,2.65));
#24494=CARTESIAN_POINT('Ctrl Pts',(-5.29999999999999,19.1973684210526,1.42013071988495));
#24495=CARTESIAN_POINT('Ctrl Pts',(-5.29999999999999,19.3947368421053,3.2453140177324E-16));
#24496=CARTESIAN_POINT('Ctrl Pts',(-5.29999999999999,19.5921052631579,-1.42013071988495));
#24497=CARTESIAN_POINT('Ctrl Pts',(-4.58993464005752,19.7894736842105,-2.64999999999999));
#24498=CARTESIAN_POINT('Ctrl Pts',(-3.87986928011504,19.9868421052632,-3.87986928011504));
#24499=CARTESIAN_POINT('Ctrl Pts',(-2.65,20.1842105263158,-4.58993464005752));
#24500=CARTESIAN_POINT('Ctrl Pts',(-1.42013071988495,20.3815789473684,-5.29999999999999));
#24501=CARTESIAN_POINT('Ctrl Pts',(-6.49062803547903E-16,20.578947368421,
-5.29999999999999));
#24502=CARTESIAN_POINT('Ctrl Pts',(1.42013071988495,20.7763157894736,-5.29999999999999));
#24503=CARTESIAN_POINT('Ctrl Pts',(2.65,20.9736842105263,-4.58993464005752));
#24504=CARTESIAN_POINT('Ctrl Pts',(3.87986928011504,21.171052631579,-3.87986928011504));
#24505=CARTESIAN_POINT('Ctrl Pts',(4.58993464005752,21.3684210526315,-2.65));
#24506=CARTESIAN_POINT('Ctrl Pts',(5.29999999999999,21.5657894736842,-1.42013071988495));
#24507=CARTESIAN_POINT('Ctrl Pts',(5.29999999999999,21.7631578947368,-9.73594205321327E-16));
#24508=CARTESIAN_POINT('Ctrl Pts',(5.29999999999999,21.9605263157895,1.42013071988495));
#24509=CARTESIAN_POINT('Ctrl Pts',(4.58993464005752,22.1578947368421,2.64999999999999));
#24510=CARTESIAN_POINT('Ctrl Pts',(3.87986928011504,22.3552631578947,3.87986928011504));
#24511=CARTESIAN_POINT('Ctrl Pts',(2.65,22.5526315789474,4.58993464005752));
#24512=CARTESIAN_POINT('Ctrl Pts',(1.42013071988495,22.75,5.29999999999999));
#24513=CARTESIAN_POINT('Ctrl Pts',(2.77333911991762E-28,22.9473684210526,
5.29999999999999));
#24514=CARTESIAN_POINT('Ctrl Pts',(-1.42013071988495,23.1447368421053,5.29999999999999));
#24515=CARTESIAN_POINT('Ctrl Pts',(-2.65,23.3421052631579,4.58993464005752));
#24516=CARTESIAN_POINT('Ctrl Pts',(-3.87986928011504,23.5394736842105,3.87986928011504));
#24517=CARTESIAN_POINT('Ctrl Pts',(-4.58993464005752,23.7368421052632,2.65));
#24518=CARTESIAN_POINT('Ctrl Pts',(-5.29999999999999,23.9342105263158,1.42013071988495));
#24519=CARTESIAN_POINT('Ctrl Pts',(-5.29999999999999,24.1315789473684,3.2453140177324E-16));
#24520=CARTESIAN_POINT('Ctrl Pts',(-5.29999999999999,24.328947368421,-1.42013071988495));
#24521=CARTESIAN_POINT('Ctrl Pts',(-4.58993464005752,24.5263157894737,-2.65));
#24522=CARTESIAN_POINT('Ctrl Pts',(-3.87986928011504,24.7236842105263,-3.87986928011504));
#24523=CARTESIAN_POINT('Ctrl Pts',(-2.65,24.9210526315789,-4.58993464005752));
#24524=CARTESIAN_POINT('Ctrl Pts',(-1.42013071988495,25.1184210526316,-5.29999999999999));
#24525=CARTESIAN_POINT('Ctrl Pts',(-6.49062803547847E-16,25.3157894736842,
-5.3));
#24526=CARTESIAN_POINT('Ctrl Pts',(1.42013071988495,25.5131578947368,-5.29999999999999));
#24527=CARTESIAN_POINT('Ctrl Pts',(2.65,25.7105263157895,-4.58993464005752));
#24528=CARTESIAN_POINT('Ctrl Pts',(3.87986928011504,25.9078947368421,-3.87986928011504));
#24529=CARTESIAN_POINT('Ctrl Pts',(4.58993464005752,26.1052631578947,-2.65));
#24530=CARTESIAN_POINT('Ctrl Pts',(5.29999999999999,26.3026315789474,-1.42013071988495));
#24531=CARTESIAN_POINT('Ctrl Pts',(5.29999999999999,26.5,-9.73594205321327E-16));
#24532=CARTESIAN_POINT('Ctrl Pts',(5.29999999999999,26.6973684210526,1.42013071988495));
#24533=CARTESIAN_POINT('Ctrl Pts',(4.58993464005752,26.8947368421053,2.64999999999999));
#24534=CARTESIAN_POINT('Ctrl Pts',(3.87986928011504,27.0921052631579,3.87986928011504));
#24535=CARTESIAN_POINT('Ctrl Pts',(2.65,27.2894736842106,4.58993464005751));
#24536=CARTESIAN_POINT('Ctrl Pts',(1.42013071988495,27.4868421052632,5.29999999999999));
#24537=CARTESIAN_POINT('Ctrl Pts',(3.33956252356747E-28,27.6842105263158,
5.29999999999999));
#24538=CARTESIAN_POINT('Ctrl Pts',(-1.42013071988495,27.8815789473684,5.29999999999999));
#24539=CARTESIAN_POINT('Ctrl Pts',(-2.65,28.0789473684211,4.58993464005751));
#24540=CARTESIAN_POINT('Ctrl Pts',(-3.87986928011504,28.2763157894737,3.87986928011504));
#24541=CARTESIAN_POINT('Ctrl Pts',(-4.58993464005752,28.4736842105263,2.65));
#24542=CARTESIAN_POINT('Ctrl Pts',(-5.29999999999999,28.671052631579,1.42013071988495));
#24543=CARTESIAN_POINT('Ctrl Pts',(-5.29999999999999,28.8684210526316,3.24531401773092E-16));
#24544=CARTESIAN_POINT('Ctrl Pts',(-5.29999999999999,29.0657894736842,-1.42013071988495));
#24545=CARTESIAN_POINT('Ctrl Pts',(-4.58993464005752,29.2631578947368,-2.65));
#24546=CARTESIAN_POINT('Ctrl Pts',(-3.87986928011504,29.4605263157895,-3.87986928011504));
#24547=CARTESIAN_POINT('Ctrl Pts',(-2.65,29.6578947368421,-4.58993464005752));
#24548=CARTESIAN_POINT('Ctrl Pts',(-1.42013071988495,29.8552631578947,-5.29999999999999));
#24549=CARTESIAN_POINT('Ctrl Pts',(-6.49062803547792E-16,30.0526315789473,
-5.29999999999999));
#24550=CARTESIAN_POINT('Ctrl Pts',(1.42013071988495,30.25,-5.29999999999999));
#24551=CARTESIAN_POINT('Ctrl Pts',(2.65,30.4473684210526,-4.58993464005752));
#24552=CARTESIAN_POINT('Ctrl Pts',(3.87986928011504,30.6447368421052,-3.87986928011504));
#24553=CARTESIAN_POINT('Ctrl Pts',(4.58993464005752,30.8421052631579,-2.65));
#24554=CARTESIAN_POINT('Ctrl Pts',(5.29999999999999,31.0394736842105,-1.42013071988495));
#24555=CARTESIAN_POINT('Ctrl Pts',(5.29999999999999,31.2368421052632,-9.73594205321327E-16));
#24556=CARTESIAN_POINT('Ctrl Pts',(5.29999999999999,31.4342105263158,1.42013071988495));
#24557=CARTESIAN_POINT('Ctrl Pts',(4.58993464005752,31.6315789473684,2.64999999999999));
#24558=CARTESIAN_POINT('Ctrl Pts',(3.87986928011504,31.8289473684211,3.87986928011504));
#24559=CARTESIAN_POINT('Ctrl Pts',(2.65,32.0263157894737,4.58993464005751));
#24560=CARTESIAN_POINT('Ctrl Pts',(1.42013071988495,32.2236842105263,5.29999999999999));
#24561=CARTESIAN_POINT('Ctrl Pts',(3.87111918821834E-28,32.421052631579,
5.29999999999999));
#24562=CARTESIAN_POINT('Ctrl Pts',(-1.42013071988495,32.6184210526316,5.29999999999999));
#24563=CARTESIAN_POINT('Ctrl Pts',(-2.65,32.8157894736842,4.58993464005752));
#24564=CARTESIAN_POINT('Ctrl Pts',(-3.87986928011504,33.0131578947369,3.87986928011504));
#24565=CARTESIAN_POINT('Ctrl Pts',(-4.58993464005752,33.2105263157895,2.65));
#24566=CARTESIAN_POINT('Ctrl Pts',(-5.29999999999999,33.4078947368421,1.42013071988495));
#24567=CARTESIAN_POINT('Ctrl Pts',(-5.29999999999999,33.6052631578947,3.24531401773092E-16));
#24568=CARTESIAN_POINT('Ctrl Pts',(-5.29999999999999,33.8026315789473,-1.42013071988495));
#24569=CARTESIAN_POINT('Ctrl Pts',(-4.58993464005752,34.,-2.65));
#24570=CARTESIAN_POINT('Ctrl Pts',(-3.87986928011504,34.1973684210526,-3.87986928011504));
#24571=CARTESIAN_POINT('Ctrl Pts',(-2.65,34.3947368421052,-4.58993464005752));
#24572=CARTESIAN_POINT('Ctrl Pts',(-1.42013071988495,34.5921052631579,-5.29999999999999));
#24573=CARTESIAN_POINT('Ctrl Pts',(-6.49062803547743E-16,34.7894736842105,
-5.3));
#24574=CARTESIAN_POINT('Ctrl Pts',(1.42013071988495,34.9868421052631,-5.29999999999999));
#24575=CARTESIAN_POINT('Ctrl Pts',(2.65,35.1842105263157,-4.58993464005752));
#24576=CARTESIAN_POINT('Ctrl Pts',(3.87986928011504,35.3815789473684,-3.87986928011505));
#24577=CARTESIAN_POINT('Ctrl Pts',(4.58993464005752,35.578947368421,-2.65));
#24578=CARTESIAN_POINT('Ctrl Pts',(5.29999999999999,35.7763157894737,-1.42013071988495));
#24579=CARTESIAN_POINT('Ctrl Pts',(5.29999999999999,35.9736842105263,-9.73594205321179E-16));
#24580=CARTESIAN_POINT('Ctrl Pts',(5.29999999999999,36.171052631579,1.42013071988494));
#24581=CARTESIAN_POINT('Ctrl Pts',(4.58993464005752,36.3684210526316,2.64999999999999));
#24582=CARTESIAN_POINT('Ctrl Pts',(3.87986928011504,36.5657894736842,3.87986928011504));
#24583=CARTESIAN_POINT('Ctrl Pts',(2.65,36.7631578947368,4.58993464005752));
#24584=CARTESIAN_POINT('Ctrl Pts',(1.42013071988495,36.9605263157895,5.29999999999999));
#24585=CARTESIAN_POINT('Ctrl Pts',(4.36800911387025E-28,37.1578947368421,
5.29999999999999));
#24586=CARTESIAN_POINT('Ctrl Pts',(-1.42013071988495,37.3552631578947,5.29999999999999));
#24587=CARTESIAN_POINT('Ctrl Pts',(-2.65,37.5526315789474,4.58993464005752));
#24588=CARTESIAN_POINT('Ctrl Pts',(-3.87986928011504,37.75,3.87986928011504));
#24589=CARTESIAN_POINT('Ctrl Pts',(-4.58993464005752,37.9473684210526,2.65));
#24590=CARTESIAN_POINT('Ctrl Pts',(-5.29999999999999,38.1447368421053,1.42013071988495));
#24591=CARTESIAN_POINT('Ctrl Pts',(-5.29999999999999,38.3421052631579,3.2453140177324E-16));
#24592=CARTESIAN_POINT('Ctrl Pts',(-5.29999999999999,38.5394736842105,-1.42013071988495));
#24593=CARTESIAN_POINT('Ctrl Pts',(-4.58993464005752,38.7368421052632,-2.65));
#24594=CARTESIAN_POINT('Ctrl Pts',(-3.87986928011504,38.9342105263158,-3.87986928011504));
#24595=CARTESIAN_POINT('Ctrl Pts',(-2.65,39.1315789473684,-4.58993464005752));
#24596=CARTESIAN_POINT('Ctrl Pts',(-1.42013071988495,39.328947368421,-5.29999999999999));
#24597=CARTESIAN_POINT('Ctrl Pts',(-6.49062803547689E-16,39.5263157894736,
-5.29999999999999));
#24598=CARTESIAN_POINT('Ctrl Pts',(1.42013071988495,39.7236842105263,-5.29999999999999));
#24599=CARTESIAN_POINT('Ctrl Pts',(2.65,39.9210526315789,-4.58993464005752));
#24600=CARTESIAN_POINT('Ctrl Pts',(3.87986928011504,40.1184210526316,-3.87986928011504));
#24601=CARTESIAN_POINT('Ctrl Pts',(4.58993464005752,40.3157894736842,-2.65));
#24602=CARTESIAN_POINT('Ctrl Pts',(5.29999999999999,40.5131578947368,-1.42013071988495));
#24603=CARTESIAN_POINT('Ctrl Pts',(5.29999999999999,40.7105263157895,-9.73594205321179E-16));
#24604=CARTESIAN_POINT('Ctrl Pts',(5.29999999999999,40.9078947368421,1.42013071988495));
#24605=CARTESIAN_POINT('Ctrl Pts',(4.58993464005752,41.1052631578947,2.64999999999999));
#24606=CARTESIAN_POINT('Ctrl Pts',(3.87986928011504,41.3026315789474,3.87986928011504));
#24607=CARTESIAN_POINT('Ctrl Pts',(2.65,41.5,4.58993464005751));
#24608=CARTESIAN_POINT('Ctrl Pts',(1.42013071988495,41.6973684210527,5.29999999999999));
#24609=CARTESIAN_POINT('Ctrl Pts',(4.92267693785377E-28,41.8947368421053,
5.29999999999999));
#24610=CARTESIAN_POINT('Ctrl Pts',(-1.42013071988495,42.0921052631579,5.29999999999999));
#24611=CARTESIAN_POINT('Ctrl Pts',(-2.65,42.2894736842105,4.58993464005752));
#24612=CARTESIAN_POINT('Ctrl Pts',(-3.87986928011504,42.4868421052632,3.87986928011504));
#24613=CARTESIAN_POINT('Ctrl Pts',(-4.58993464005752,42.6842105263158,2.65));
#24614=CARTESIAN_POINT('Ctrl Pts',(-5.29999999999999,42.8815789473684,1.42013071988495));
#24615=CARTESIAN_POINT('Ctrl Pts',(-5.29999999999999,43.078947368421,3.2453140177324E-16));
#24616=CARTESIAN_POINT('Ctrl Pts',(-5.29999999999999,43.2763157894737,-1.42013071988495));
#24617=CARTESIAN_POINT('Ctrl Pts',(-4.58993464005752,43.4736842105263,-2.64999999999999));
#24618=CARTESIAN_POINT('Ctrl Pts',(-3.87986928011504,43.6710526315789,-3.87986928011504));
#24619=CARTESIAN_POINT('Ctrl Pts',(-2.65,43.8684210526316,-4.58993464005752));
#24620=CARTESIAN_POINT('Ctrl Pts',(-1.42013071988495,44.0657894736842,-5.29999999999999));
#24621=CARTESIAN_POINT('Ctrl Pts',(-6.4906280354764E-16,44.2631578947368,
-5.3));
#24622=CARTESIAN_POINT('Ctrl Pts',(1.42013071988495,44.4605263157895,-5.29999999999999));
#24623=CARTESIAN_POINT('Ctrl Pts',(2.65,44.6578947368421,-4.58993464005752));
#24624=CARTESIAN_POINT('Ctrl Pts',(3.87986928011504,44.8552631578947,-3.87986928011504));
#24625=CARTESIAN_POINT('Ctrl Pts',(4.58993464005752,45.0526315789473,-2.65));
#24626=CARTESIAN_POINT('Ctrl Pts',(5.29999999999999,45.25,-1.42013071988495));
#24627=CARTESIAN_POINT('Ctrl Pts',(5.29999999999999,45.4473684210526,-9.73594205321327E-16));
#24628=CARTESIAN_POINT('Ctrl Pts',(5.29999999999999,45.6447368421053,1.42013071988495));
#24629=CARTESIAN_POINT('Ctrl Pts',(4.58993464005752,45.8421052631579,2.64999999999999));
#24630=CARTESIAN_POINT('Ctrl Pts',(3.87986928011504,46.0394736842105,3.87986928011504));
#24631=CARTESIAN_POINT('Ctrl Pts',(2.65,46.2368421052632,4.58993464005752));
#24632=CARTESIAN_POINT('Ctrl Pts',(1.42013071988495,46.4342105263158,5.29999999999999));
#24633=CARTESIAN_POINT('Ctrl Pts',(5.40801128383936E-28,46.6315789473685,
5.29999999999999));
#24634=CARTESIAN_POINT('Ctrl Pts',(-1.42013071988495,46.8289473684211,5.29999999999999));
#24635=CARTESIAN_POINT('Ctrl Pts',(-2.65,47.0263157894737,4.58993464005752));
#24636=CARTESIAN_POINT('Ctrl Pts',(-3.87986928011504,47.2236842105263,3.87986928011504));
#24637=CARTESIAN_POINT('Ctrl Pts',(-4.58993464005752,47.421052631579,2.65));
#24638=CARTESIAN_POINT('Ctrl Pts',(-5.29999999999999,47.6184210526316,1.42013071988495));
#24639=CARTESIAN_POINT('Ctrl Pts',(-5.29999999999999,47.8157894736842,3.2453140177324E-16));
#24640=CARTESIAN_POINT('Ctrl Pts',(-5.29999999999999,48.0131578947369,-1.42013071988495));
#24641=CARTESIAN_POINT('Ctrl Pts',(-4.58993464005752,48.2105263157895,-2.64999999999999));
#24642=CARTESIAN_POINT('Ctrl Pts',(-3.87986928011504,48.4078947368421,-3.87986928011504));
#24643=CARTESIAN_POINT('Ctrl Pts',(-2.65,48.6052631578947,-4.58993464005752));
#24644=CARTESIAN_POINT('Ctrl Pts',(-1.42013071988495,48.8026315789473,-5.29999999999999));
#24645=CARTESIAN_POINT('Ctrl Pts',(-6.49062803547591E-16,49.,-5.29999999999999));
#24646=CARTESIAN_POINT('Ctrl Pts',(1.42013071988495,49.1973684210526,-5.29999999999999));
#24647=CARTESIAN_POINT('Ctrl Pts',(2.65,49.3947368421053,-4.58993464005752));
#24648=CARTESIAN_POINT('Ctrl Pts',(3.87986928011504,49.5921052631579,-3.87986928011504));
#24649=CARTESIAN_POINT('Ctrl Pts',(4.58993464005752,49.7894736842105,-2.65));
#24650=CARTESIAN_POINT('Ctrl Pts',(5.29999999999999,49.9868421052632,-1.42013071988495));
#24651=CARTESIAN_POINT('Ctrl Pts',(5.29999999999999,50.1842105263158,-9.73594205321327E-16));
#24652=CARTESIAN_POINT('Ctrl Pts',(5.29999999999999,50.3815789473684,1.42013071988495));
#24653=CARTESIAN_POINT('Ctrl Pts',(4.58993464005752,50.5789473684211,2.64999999999999));
#24654=CARTESIAN_POINT('Ctrl Pts',(3.87986928011504,50.7763157894737,3.87986928011504));
#24655=CARTESIAN_POINT('Ctrl Pts',(2.65,50.9736842105264,4.58993464005751));
#24656=CARTESIAN_POINT('Ctrl Pts',(1.42013071988495,51.171052631579,5.29999999999999));
#24657=CARTESIAN_POINT('Ctrl Pts',(5.90490120949126E-28,51.3684210526317,
5.29999999999999));
#24658=CARTESIAN_POINT('Ctrl Pts',(-1.42013071988495,51.5657894736843,5.29999999999999));
#24659=CARTESIAN_POINT('Ctrl Pts',(-2.65,51.7631578947368,4.58993464005751));
#24660=CARTESIAN_POINT('Ctrl Pts',(-3.87986928011504,51.9605263157895,3.87986928011504));
#24661=CARTESIAN_POINT('Ctrl Pts',(-4.58993464005752,52.1578947368421,2.65));
#24662=CARTESIAN_POINT('Ctrl Pts',(-5.29999999999999,52.3552631578947,1.42013071988495));
#24663=CARTESIAN_POINT('Ctrl Pts',(-5.29999999999999,52.5526315789474,3.24531401773979E-16));
#24664=CARTESIAN_POINT('Ctrl Pts',(-5.29999999999999,52.75,-1.42013071988495));
#24665=CARTESIAN_POINT('Ctrl Pts',(-4.58993464005752,52.9473684210526,-2.65));
#24666=CARTESIAN_POINT('Ctrl Pts',(-3.87986928011504,53.1447368421053,-3.87986928011504));
#24667=CARTESIAN_POINT('Ctrl Pts',(-2.65,53.3421052631578,-4.58993464005752));
#24668=CARTESIAN_POINT('Ctrl Pts',(-1.42013071988495,53.5394736842104,-5.29999999999999));
#24669=CARTESIAN_POINT('Ctrl Pts',(-6.49062803547537E-16,53.7368421052631,
-5.29999999999999));
#24670=CARTESIAN_POINT('Ctrl Pts',(1.42013071988495,53.9342105263157,-5.29999999999999));
#24671=CARTESIAN_POINT('Ctrl Pts',(2.65,54.1315789473684,-4.58993464005752));
#24672=CARTESIAN_POINT('Ctrl Pts',(3.87986928011504,54.3289473684211,-3.87986928011504));
#24673=CARTESIAN_POINT('Ctrl Pts',(4.58993464005752,54.5263157894736,-2.65));
#24674=CARTESIAN_POINT('Ctrl Pts',(5.29999999999999,54.7236842105263,-1.42013071988495));
#24675=CARTESIAN_POINT('Ctrl Pts',(5.29999999999999,54.9210526315789,-9.73594205321327E-16));
#24676=CARTESIAN_POINT('Ctrl Pts',(5.29999999999999,55.1184210526316,1.42013071988495));
#24677=CARTESIAN_POINT('Ctrl Pts',(4.58993464005752,55.3157894736842,2.64999999999999));
#24678=CARTESIAN_POINT('Ctrl Pts',(3.87986928011504,55.5131578947368,3.87986928011504));
#24679=CARTESIAN_POINT('Ctrl Pts',(2.65,55.7105263157895,4.58993464005752));
#24680=CARTESIAN_POINT('Ctrl Pts',(1.42013071988495,55.9078947368422,5.29999999999999));
#24681=CARTESIAN_POINT('Ctrl Pts',(6.44801345380847E-28,56.1052631578948,
5.29999999999999));
#24682=CARTESIAN_POINT('Ctrl Pts',(-1.42013071988495,56.3026315789474,5.29999999999999));
#24683=CARTESIAN_POINT('Ctrl Pts',(-2.65,56.5000000000001,4.58993464005752));
#24684=CARTESIAN_POINT('Ctrl Pts',(-3.87986928011504,56.6973684210526,3.87986928011504));
#24685=CARTESIAN_POINT('Ctrl Pts',(-4.58993464005752,56.8947368421053,2.65));
#24686=CARTESIAN_POINT('Ctrl Pts',(-5.29999999999999,57.0921052631579,1.42013071988495));
#24687=CARTESIAN_POINT('Ctrl Pts',(-5.29999999999999,57.2894736842105,3.24531401773979E-16));
#24688=CARTESIAN_POINT('Ctrl Pts',(-5.29999999999999,57.4868421052631,-1.42013071988495));
#24689=CARTESIAN_POINT('Ctrl Pts',(-4.58993464005752,57.6842105263158,-2.65));
#24690=CARTESIAN_POINT('Ctrl Pts',(-3.87986928011504,57.8815789473684,-3.87986928011504));
#24691=CARTESIAN_POINT('Ctrl Pts',(-2.65,58.078947368421,-4.58993464005752));
#24692=CARTESIAN_POINT('Ctrl Pts',(-1.42013071988495,58.2763157894737,-5.29999999999999));
#24693=CARTESIAN_POINT('Ctrl Pts',(-6.49062803547481E-16,58.4736842105263,
-5.3));
#24694=CARTESIAN_POINT('Ctrl Pts',(1.42013071988495,58.6710526315789,-5.29999999999999));
#24695=CARTESIAN_POINT('Ctrl Pts',(2.65,58.8684210526315,-4.58993464005752));
#24696=CARTESIAN_POINT('Ctrl Pts',(3.87986928011504,59.0657894736842,-3.87986928011504));
#24697=CARTESIAN_POINT('Ctrl Pts',(4.58993464005752,59.2631578947368,-2.65));
#24698=CARTESIAN_POINT('Ctrl Pts',(5.29999999999999,59.4605263157895,-1.42013071988495));
#24699=CARTESIAN_POINT('Ctrl Pts',(5.29999999999999,59.6578947368421,-9.73594205321179E-16));
#24700=CARTESIAN_POINT('Ctrl Pts',(5.29999999999999,59.8552631578947,1.42013071988494));
#24701=CARTESIAN_POINT('Ctrl Pts',(4.58993464005752,60.0526315789474,2.64999999999999));
#24702=CARTESIAN_POINT('Ctrl Pts',(3.87986928011504,60.25,3.87986928011504));
#24703=CARTESIAN_POINT('Ctrl Pts',(2.65,60.4473684210527,4.58993464005752));
#24704=CARTESIAN_POINT('Ctrl Pts',(1.42013071988495,60.6447368421053,5.29999999999999));
#24705=CARTESIAN_POINT('Ctrl Pts',(7.00268127779199E-28,60.8421052631579,
5.29999999999999));
#24706=CARTESIAN_POINT('Ctrl Pts',(-1.42013071988495,61.0394736842105,5.29999999999999));
#24707=CARTESIAN_POINT('Ctrl Pts',(-2.65,61.2368421052632,4.58993464005751));
#24708=CARTESIAN_POINT('Ctrl Pts',(-3.87986928011504,61.4342105263158,3.87986928011505));
#24709=CARTESIAN_POINT('Ctrl Pts',(-4.58993464005752,61.6315789473684,2.65));
#24710=CARTESIAN_POINT('Ctrl Pts',(-5.29999999999999,61.828947368421,1.42013071988495));
#24711=CARTESIAN_POINT('Ctrl Pts',(-5.29999999999999,62.0263157894737,3.24531401773831E-16));
#24712=CARTESIAN_POINT('Ctrl Pts',(-5.29999999999999,62.2236842105263,-1.42013071988495));
#24713=CARTESIAN_POINT('Ctrl Pts',(-4.58993464005752,62.4210526315789,-2.65));
#24714=CARTESIAN_POINT('Ctrl Pts',(-3.87986928011504,62.6184210526316,-3.87986928011504));
#24715=CARTESIAN_POINT('Ctrl Pts',(-2.65,62.8157894736841,-4.58993464005752));
#24716=CARTESIAN_POINT('Ctrl Pts',(-1.42013071988495,63.0131578947368,-5.29999999999999));
#24717=CARTESIAN_POINT('Ctrl Pts',(-6.49062803547431E-16,63.2105263157894,
-5.29999999999999));
#24718=CARTESIAN_POINT('Ctrl Pts',(1.42013071988495,63.407894736842,-5.29999999999999));
#24719=CARTESIAN_POINT('Ctrl Pts',(2.65,63.6052631578947,-4.58993464005752));
#24720=CARTESIAN_POINT('Ctrl Pts',(3.87986928011504,63.8026315789474,-3.87986928011504));
#24721=CARTESIAN_POINT('Ctrl Pts',(4.58993464005752,64.,-2.65));
#24722=CARTESIAN_POINT('Ctrl Pts',(5.29999999999999,64.1973684210526,-1.42013071988495));
#24723=CARTESIAN_POINT('Ctrl Pts',(5.29999999999999,64.3947368421052,-9.73594205321179E-16));
#24724=CARTESIAN_POINT('Ctrl Pts',(5.29999999999999,64.5921052631579,1.42013071988495));
#24725=CARTESIAN_POINT('Ctrl Pts',(4.58993464005752,64.7894736842105,2.64999999999999));
#24726=CARTESIAN_POINT('Ctrl Pts',(3.87986928011504,64.9868421052632,3.87986928011504));
#24727=CARTESIAN_POINT('Ctrl Pts',(2.65,65.1842105263158,4.58993464005751));
#24728=CARTESIAN_POINT('Ctrl Pts',(1.42013071988495,65.3815789473685,5.29999999999999));
#24729=CARTESIAN_POINT('Ctrl Pts',(7.41868214577963E-28,65.5789473684211,
5.29999999999999));
#24730=CARTESIAN_POINT('Ctrl Pts',(-1.42013071988495,65.7763157894737,5.29999999999999));
#24731=CARTESIAN_POINT('Ctrl Pts',(-2.65,65.9736842105264,4.58993464005752));
#24732=CARTESIAN_POINT('Ctrl Pts',(-3.87986928011504,66.1710526315789,3.87986928011504));
#24733=CARTESIAN_POINT('Ctrl Pts',(-4.58993464005752,66.3684210526316,2.65));
#24734=CARTESIAN_POINT('Ctrl Pts',(-5.29999999999999,66.5657894736842,1.42013071988495));
#24735=CARTESIAN_POINT('Ctrl Pts',(-5.29999999999999,66.7631578947368,3.24531401773831E-16));
#24736=CARTESIAN_POINT('Ctrl Pts',(-5.29999999999999,66.9605263157895,-1.42013071988495));
#24737=CARTESIAN_POINT('Ctrl Pts',(-4.58993464005752,67.1578947368421,-2.65));
#24738=CARTESIAN_POINT('Ctrl Pts',(-3.87986928011504,67.3552631578947,-3.87986928011504));
#24739=CARTESIAN_POINT('Ctrl Pts',(-2.65,67.5526315789473,-4.58993464005752));
#24740=CARTESIAN_POINT('Ctrl Pts',(-1.42013071988495,67.75,-5.29999999999999));
#24741=CARTESIAN_POINT('Ctrl Pts',(-6.49062803547383E-16,67.9473684210526,
-5.3));
#24742=CARTESIAN_POINT('Ctrl Pts',(1.42013071988495,68.1447368421052,-5.29999999999999));
#24743=CARTESIAN_POINT('Ctrl Pts',(2.65,68.3421052631578,-4.58993464005752));
#24744=CARTESIAN_POINT('Ctrl Pts',(3.87986928011504,68.5394736842105,-3.87986928011504));
#24745=CARTESIAN_POINT('Ctrl Pts',(4.58993464005752,68.7368421052631,-2.65));
#24746=CARTESIAN_POINT('Ctrl Pts',(5.29999999999999,68.9342105263158,-1.42013071988495));
#24747=CARTESIAN_POINT('Ctrl Pts',(5.29999999999999,69.1315789473684,-9.73594205321179E-16));
#24748=CARTESIAN_POINT('Ctrl Pts',(5.29999999999999,69.3289473684211,1.42013071988495));
#24749=CARTESIAN_POINT('Ctrl Pts',(4.58993464005752,69.5263157894736,2.64999999999999));
#24750=CARTESIAN_POINT('Ctrl Pts',(3.87986928011504,69.7236842105263,3.87986928011504));
#24751=CARTESIAN_POINT('Ctrl Pts',(2.65,69.9210526315789,4.58993464005752));
#24752=CARTESIAN_POINT('Ctrl Pts',(1.42013071988495,70.1184210526316,5.29999999999999));
#24753=CARTESIAN_POINT('Ctrl Pts',(7.97334996976316E-28,70.3157894736842,
5.29999999999999));
#24754=CARTESIAN_POINT('Ctrl Pts',(-1.42013071988495,70.5131578947368,5.29999999999999));
#24755=CARTESIAN_POINT('Ctrl Pts',(-2.65,70.7105263157895,4.58993464005752));
#24756=CARTESIAN_POINT('Ctrl Pts',(-3.87986928011504,70.9078947368421,3.87986928011504));
#24757=CARTESIAN_POINT('Ctrl Pts',(-4.58993464005752,71.1052631578947,2.65));
#24758=CARTESIAN_POINT('Ctrl Pts',(-5.29999999999999,71.3026315789474,1.42013071988495));
#24759=CARTESIAN_POINT('Ctrl Pts',(-5.29999999999999,71.5,3.24531401773831E-16));
#24760=CARTESIAN_POINT('Ctrl Pts',(-5.29999999999999,71.6973684210526,-1.42013071988495));
#24761=CARTESIAN_POINT('Ctrl Pts',(-4.58993464005752,71.8947368421052,-2.65));
#24762=CARTESIAN_POINT('Ctrl Pts',(-3.87986928011504,72.0921052631579,-3.87986928011504));
#24763=CARTESIAN_POINT('Ctrl Pts',(-2.65,72.2894736842104,-4.58993464005752));
#24764=CARTESIAN_POINT('Ctrl Pts',(-1.42013071988495,72.4868421052631,-5.29999999999999));
#24765=CARTESIAN_POINT('Ctrl Pts',(-6.49062803547328E-16,72.6842105263157,
-5.29999999999999));
#24766=CARTESIAN_POINT('Ctrl Pts',(1.42013071988495,72.8815789473684,-5.29999999999999));
#24767=CARTESIAN_POINT('Ctrl Pts',(2.65,73.078947368421,-4.58993464005752));
#24768=CARTESIAN_POINT('Ctrl Pts',(3.87986928011504,73.2763157894737,-3.87986928011504));
#24769=CARTESIAN_POINT('Ctrl Pts',(4.58993464005752,73.4736842105263,-2.65));
#24770=CARTESIAN_POINT('Ctrl Pts',(5.29999999999999,73.6710526315789,-1.42013071988495));
#24771=CARTESIAN_POINT('Ctrl Pts',(5.29999999999999,73.8684210526316,-9.73594205321179E-16));
#24772=CARTESIAN_POINT('Ctrl Pts',(5.29999999999999,74.0657894736842,1.42013071988495));
#24773=CARTESIAN_POINT('Ctrl Pts',(4.58993464005752,74.2631578947368,2.64999999999999));
#24774=CARTESIAN_POINT('Ctrl Pts',(3.87986928011504,74.4605263157895,3.87986928011504));
#24775=CARTESIAN_POINT('Ctrl Pts',(2.65,74.6578947368421,4.58993464005751));
#24776=CARTESIAN_POINT('Ctrl Pts',(1.42013071988495,74.8552631578948,5.29999999999999));
#24777=CARTESIAN_POINT('Ctrl Pts',(8.539573373413E-28,75.0526315789474,
5.29999999999999));
#24778=CARTESIAN_POINT('Ctrl Pts',(-1.42013071988495,75.2500000000001,5.29999999999999));
#24779=CARTESIAN_POINT('Ctrl Pts',(-2.65,75.4473684210526,4.58993464005751));
#24780=CARTESIAN_POINT('Ctrl Pts',(-3.87986928011504,75.6447368421053,3.87986928011504));
#24781=CARTESIAN_POINT('Ctrl Pts',(-4.58993464005752,75.8421052631579,2.65));
#24782=CARTESIAN_POINT('Ctrl Pts',(-5.29999999999999,76.0394736842105,1.42013071988495));
#24783=CARTESIAN_POINT('Ctrl Pts',(-5.29999999999999,76.2368421052631,3.24531401773831E-16));
#24784=CARTESIAN_POINT('Ctrl Pts',(-5.29999999999999,76.4342105263158,-1.42013071988495));
#24785=CARTESIAN_POINT('Ctrl Pts',(-4.58993464005752,76.6315789473684,-2.64999999999999));
#24786=CARTESIAN_POINT('Ctrl Pts',(-3.87986928011504,76.828947368421,-3.87986928011504));
#24787=CARTESIAN_POINT('Ctrl Pts',(-2.65,77.0263157894736,-4.58993464005752));
#24788=CARTESIAN_POINT('Ctrl Pts',(-1.42013071988495,77.2236842105262,-5.29999999999999));
#24789=CARTESIAN_POINT('Ctrl Pts',(-6.49062803547279E-16,77.4210526315788,
-5.3));
#24790=CARTESIAN_POINT('Ctrl Pts',(1.42013071988495,77.6184210526316,-5.29999999999999));
#24791=CARTESIAN_POINT('Ctrl Pts',(2.65,77.8157894736841,-4.58993464005752));
#24792=CARTESIAN_POINT('Ctrl Pts',(3.87986928011504,78.0131578947368,-3.87986928011505));
#24793=CARTESIAN_POINT('Ctrl Pts',(4.58993464005752,78.2105263157895,-2.65));
#24794=CARTESIAN_POINT('Ctrl Pts',(5.29999999999999,78.4078947368421,-1.42013071988495));
#24795=CARTESIAN_POINT('Ctrl Pts',(5.29999999999999,78.6052631578947,-9.73594205321327E-16));
#24796=CARTESIAN_POINT('Ctrl Pts',(5.29999999999999,78.8026315789474,1.42013071988494));
#24797=CARTESIAN_POINT('Ctrl Pts',(4.58993464005752,79.,2.64999999999999));
#24798=CARTESIAN_POINT('Ctrl Pts',(3.87986928011504,79.1973684210527,3.87986928011504));
#24799=CARTESIAN_POINT('Ctrl Pts',(2.65,79.3947368421053,4.58993464005752));
#24800=CARTESIAN_POINT('Ctrl Pts',(1.42013071988495,79.5921052631579,5.29999999999999));
#24801=CARTESIAN_POINT('Ctrl Pts',(9.07113003806388E-28,79.7894736842106,
5.29999999999999));
#24802=CARTESIAN_POINT('Ctrl Pts',(-1.42013071988495,79.9868421052632,5.29999999999999));
#24803=CARTESIAN_POINT('Ctrl Pts',(-2.65,80.1842105263158,4.58993464005752));
#24804=CARTESIAN_POINT('Ctrl Pts',(-3.87986928011504,80.3815789473684,3.87986928011504));
#24805=CARTESIAN_POINT('Ctrl Pts',(-4.58993464005752,80.578947368421,2.65));
#24806=CARTESIAN_POINT('Ctrl Pts',(-5.29999999999999,80.7763157894737,1.42013071988495));
#24807=CARTESIAN_POINT('Ctrl Pts',(-5.29999999999999,80.9736842105263,3.24531401773831E-16));
#24808=CARTESIAN_POINT('Ctrl Pts',(-5.29999999999999,81.171052631579,-1.42013071988495));
#24809=CARTESIAN_POINT('Ctrl Pts',(-4.58993464005752,81.3684210526315,-2.64999999999999));
#24810=CARTESIAN_POINT('Ctrl Pts',(-3.87986928011504,81.5657894736842,-3.87986928011504));
#24811=CARTESIAN_POINT('Ctrl Pts',(-2.65,81.7631578947368,-4.58993464005752));
#24812=CARTESIAN_POINT('Ctrl Pts',(-1.42013071988495,81.9605263157895,-5.29999999999999));
#24813=CARTESIAN_POINT('Ctrl Pts',(-6.49062803547223E-16,82.1578947368421,
-5.29999999999999));
#24814=CARTESIAN_POINT('Ctrl Pts',(1.42013071988495,82.3552631578947,-5.29999999999999));
#24815=CARTESIAN_POINT('Ctrl Pts',(2.65,82.5526315789474,-4.58993464005752));
#24816=CARTESIAN_POINT('Ctrl Pts',(3.87986928011504,82.75,-3.87986928011504));
#24817=CARTESIAN_POINT('Ctrl Pts',(4.58993464005752,82.9473684210526,-2.65));
#24818=CARTESIAN_POINT('Ctrl Pts',(5.29999999999999,83.1447368421053,-1.42013071988495));
#24819=CARTESIAN_POINT('Ctrl Pts',(5.29999999999999,83.3421052631579,-9.73594205321327E-16));
#24820=CARTESIAN_POINT('Ctrl Pts',(5.29999999999999,83.5394736842105,1.42013071988495));
#24821=CARTESIAN_POINT('Ctrl Pts',(4.58993464005752,83.7368421052632,2.64999999999999));
#24822=CARTESIAN_POINT('Ctrl Pts',(3.87986928011504,83.9342105263158,3.87986928011504));
#24823=CARTESIAN_POINT('Ctrl Pts',(2.65,84.1315789473685,4.58993464005751));
#24824=CARTESIAN_POINT('Ctrl Pts',(1.42013071988495,84.3289473684211,5.29999999999999));
#24825=CARTESIAN_POINT('Ctrl Pts',(9.56801996371578E-28,84.5263157894737,
5.29999999999999));
#24826=CARTESIAN_POINT('Ctrl Pts',(-1.42013071988495,84.7236842105264,5.29999999999999));
#24827=CARTESIAN_POINT('Ctrl Pts',(-2.65,84.921052631579,4.58993464005751));
#24828=CARTESIAN_POINT('Ctrl Pts',(-3.87986928011504,85.1184210526316,3.87986928011504));
#24829=CARTESIAN_POINT('Ctrl Pts',(-4.58993464005752,85.3157894736842,2.65));
#24830=CARTESIAN_POINT('Ctrl Pts',(-5.29999999999999,85.5131578947368,1.42013071988495));
#24831=CARTESIAN_POINT('Ctrl Pts',(-5.29999999999999,85.7105263157894,3.24531401773979E-16));
#24832=CARTESIAN_POINT('Ctrl Pts',(-5.29999999999999,85.9078947368421,-1.42013071988495));
#24833=CARTESIAN_POINT('Ctrl Pts',(-4.58993464005752,86.1052631578947,-2.65));
#24834=CARTESIAN_POINT('Ctrl Pts',(-3.87986928011504,86.3026315789474,-3.87986928011504));
#24835=CARTESIAN_POINT('Ctrl Pts',(-2.65,86.5,-4.58993464005752));
#24836=CARTESIAN_POINT('Ctrl Pts',(-1.42013071988495,86.6973684210525,-5.29999999999999));
#24837=CARTESIAN_POINT('Ctrl Pts',(-6.49062803547175E-16,86.8947368421052,
-5.29999999999999));
#24838=CARTESIAN_POINT('Ctrl Pts',(1.42013071988495,87.0921052631578,-5.29999999999999));
#24839=CARTESIAN_POINT('Ctrl Pts',(2.65,87.2894736842105,-4.58993464005752));
#24840=CARTESIAN_POINT('Ctrl Pts',(3.87986928011504,87.4868421052632,-3.87986928011504));
#24841=CARTESIAN_POINT('Ctrl Pts',(4.58993464005752,87.6842105263158,-2.65));
#24842=CARTESIAN_POINT('Ctrl Pts',(5.29999999999999,87.8815789473684,-1.42013071988495));
#24843=CARTESIAN_POINT('Ctrl Pts',(5.29999999999999,88.078947368421,-9.73594205322067E-16));
#24844=CARTESIAN_POINT('Ctrl Pts',(5.29999999999999,88.2763157894737,1.42013071988495));
#24845=CARTESIAN_POINT('Ctrl Pts',(4.58993464005752,88.4736842105263,2.64999999999999));
#24846=CARTESIAN_POINT('Ctrl Pts',(3.87986928011504,88.6710526315789,3.87986928011504));
#24847=CARTESIAN_POINT('Ctrl Pts',(2.65,88.8684210526316,4.58993464005752));
#24848=CARTESIAN_POINT('Ctrl Pts',(1.42013071988495,89.0657894736842,5.29999999999999));
#24849=CARTESIAN_POINT('Ctrl Pts',(1.00533543097014E-27,89.2631578947369,
5.29999999999999));
#24850=CARTESIAN_POINT('Ctrl Pts',(-1.42013071988495,89.4605263157895,5.29999999999999));
#24851=CARTESIAN_POINT('Ctrl Pts',(-2.65,89.6578947368422,4.58993464005752));
#24852=CARTESIAN_POINT('Ctrl Pts',(-3.87986928011504,89.8552631578947,3.87986928011504));
#24853=CARTESIAN_POINT('Ctrl Pts',(-4.58993464005752,90.0526315789474,2.65));
#24854=CARTESIAN_POINT('Ctrl Pts',(-5.29999999999999,90.25,1.42013071988495));
#24855=CARTESIAN_POINT('Ctrl Pts',(-5.29999999999999,90.4473684210526,3.24531401774127E-16));
#24856=CARTESIAN_POINT('Ctrl Pts',(-5.29999999999999,90.6447368421053,-1.42013071988495));
#24857=CARTESIAN_POINT('Ctrl Pts',(-4.58993464005752,90.8421052631579,-2.65));
#24858=CARTESIAN_POINT('Ctrl Pts',(-3.87986928011504,91.0394736842105,-3.87986928011504));
#24859=CARTESIAN_POINT('Ctrl Pts',(-2.65,91.2368421052631,-4.58993464005752));
#24860=CARTESIAN_POINT('Ctrl Pts',(-1.42013071988495,91.4342105263158,-5.29999999999999));
#24861=CARTESIAN_POINT('Ctrl Pts',(-6.49062803547121E-16,91.6315789473684,
-5.3));
#24862=CARTESIAN_POINT('Ctrl Pts',(1.42013071988495,91.828947368421,-5.29999999999999));
#24863=CARTESIAN_POINT('Ctrl Pts',(2.65,92.0263157894737,-4.58993464005752));
#24864=CARTESIAN_POINT('Ctrl Pts',(3.87986928011504,92.2236842105263,-3.87986928011504));
#24865=CARTESIAN_POINT('Ctrl Pts',(4.58993464005752,92.4210526315789,-2.65));
#24866=CARTESIAN_POINT('Ctrl Pts',(5.29999999999999,92.6184210526316,-1.42013071988495));
#24867=CARTESIAN_POINT('Ctrl Pts',(5.29999999999999,92.8157894736842,-9.73594205322067E-16));
#24868=CARTESIAN_POINT('Ctrl Pts',(5.29999999999999,93.0131578947368,1.42013071988495));
#24869=CARTESIAN_POINT('Ctrl Pts',(4.58993464005752,93.2105263157895,2.64999999999999));
#24870=CARTESIAN_POINT('Ctrl Pts',(3.87986928011504,93.4078947368421,3.87986928011504));
#24871=CARTESIAN_POINT('Ctrl Pts',(2.65,93.6052631578947,4.58993464005752));
#24872=CARTESIAN_POINT('Ctrl Pts',(1.42013071988495,93.8026315789474,5.29999999999999));
#24873=CARTESIAN_POINT('Ctrl Pts',(1.06080221336849E-27,94.,5.29999999999999));
#24874=CARTESIAN_POINT('Ctrl Pts',(9.70668691971167E-29,3.99999999999997,
9.29999999999999));
#24875=CARTESIAN_POINT('Ctrl Pts',(-2.49192748960944,4.19736842105264,9.29999999999998));
#24876=CARTESIAN_POINT('Ctrl Pts',(-4.64999999999999,4.39473684210525,8.05403625519527));
#24877=CARTESIAN_POINT('Ctrl Pts',(-6.80807251039054,4.59210526315785,6.80807251039054));
#24878=CARTESIAN_POINT('Ctrl Pts',(-8.05403625519527,4.78947368421054,4.64999999999999));
#24879=CARTESIAN_POINT('Ctrl Pts',(-9.29999999999998,4.98684210526316,2.49192748960944));
#24880=CARTESIAN_POINT('Ctrl Pts',(-9.29999999999999,5.18421052631578,5.69460761603425E-16));
#24881=CARTESIAN_POINT('Ctrl Pts',(-9.29999999999998,5.38157894736842,-2.49192748960943));
#24882=CARTESIAN_POINT('Ctrl Pts',(-8.05403625519527,5.57894736842102,-4.64999999999999));
#24883=CARTESIAN_POINT('Ctrl Pts',(-6.80807251039054,5.77631578947368,-6.80807251039054));
#24884=CARTESIAN_POINT('Ctrl Pts',(-4.65,5.97368421052634,-8.05403625519526));
#24885=CARTESIAN_POINT('Ctrl Pts',(-2.49192748960944,6.17105263157895,-9.29999999999998));
#24886=CARTESIAN_POINT('Ctrl Pts',(-1.13892152320701E-15,6.36842105263158,
-9.29999999999999));
#24887=CARTESIAN_POINT('Ctrl Pts',(2.49192748960943,6.56578947368421,-9.29999999999999));
#24888=CARTESIAN_POINT('Ctrl Pts',(4.64999999999999,6.76315789473686,-8.05403625519527));
#24889=CARTESIAN_POINT('Ctrl Pts',(6.80807251039054,6.96052631578947,-6.80807251039055));
#24890=CARTESIAN_POINT('Ctrl Pts',(8.05403625519526,7.1578947368421,-4.65));
#24891=CARTESIAN_POINT('Ctrl Pts',(9.29999999999998,7.35526315789473,-2.49192748960945));
#24892=CARTESIAN_POINT('Ctrl Pts',(9.29999999999999,7.55263157894738,-1.70838228481055E-15));
#24893=CARTESIAN_POINT('Ctrl Pts',(9.29999999999999,7.75,2.49192748960943));
#24894=CARTESIAN_POINT('Ctrl Pts',(8.05403625519527,7.94736842105266,4.64999999999998));
#24895=CARTESIAN_POINT('Ctrl Pts',(6.80807251039055,8.14473684210526,6.80807251039054));
#24896=CARTESIAN_POINT('Ctrl Pts',(4.65,8.3421052631579,8.05403625519527));
#24897=CARTESIAN_POINT('Ctrl Pts',(2.49192748960945,8.53947368421052,9.29999999999998));
#24898=CARTESIAN_POINT('Ctrl Pts',(1.38666955995881E-28,8.73684210526314,
9.29999999999999));
#24899=CARTESIAN_POINT('Ctrl Pts',(-2.49192748960944,8.93421052631578,9.29999999999998));
#24900=CARTESIAN_POINT('Ctrl Pts',(-4.64999999999999,9.13157894736842,8.05403625519527));
#24901=CARTESIAN_POINT('Ctrl Pts',(-6.80807251039054,9.32894736842104,6.80807251039054));
#24902=CARTESIAN_POINT('Ctrl Pts',(-8.05403625519527,9.5263157894737,4.64999999999999));
#24903=CARTESIAN_POINT('Ctrl Pts',(-9.29999999999998,9.7236842105263,2.49192748960944));
#24904=CARTESIAN_POINT('Ctrl Pts',(-9.29999999999999,9.92105263157894,5.69460761603425E-16));
#24905=CARTESIAN_POINT('Ctrl Pts',(-9.29999999999998,10.1184210526316,-2.49192748960944));
#24906=CARTESIAN_POINT('Ctrl Pts',(-8.05403625519527,10.3157894736842,-4.64999999999999));
#24907=CARTESIAN_POINT('Ctrl Pts',(-6.80807251039054,10.5131578947369,-6.80807251039054));
#24908=CARTESIAN_POINT('Ctrl Pts',(-4.65,10.7105263157895,-8.05403625519526));
#24909=CARTESIAN_POINT('Ctrl Pts',(-2.49192748960944,10.9078947368421,-9.29999999999998));
#24910=CARTESIAN_POINT('Ctrl Pts',(-1.13892152320697E-15,11.1052631578947,
-9.29999999999999));
#24911=CARTESIAN_POINT('Ctrl Pts',(2.49192748960943,11.3026315789474,-9.29999999999999));
#24912=CARTESIAN_POINT('Ctrl Pts',(4.64999999999999,11.5,-8.05403625519527));
#24913=CARTESIAN_POINT('Ctrl Pts',(6.80807251039054,11.6973684210527,-6.80807251039055));
#24914=CARTESIAN_POINT('Ctrl Pts',(8.05403625519526,11.8947368421053,-4.65));
#24915=CARTESIAN_POINT('Ctrl Pts',(9.29999999999998,12.0921052631579,-2.49192748960945));
#24916=CARTESIAN_POINT('Ctrl Pts',(9.29999999999999,12.2894736842105,-1.70838228481055E-15));
#24917=CARTESIAN_POINT('Ctrl Pts',(9.29999999999999,12.4868421052632,2.49192748960943));
#24918=CARTESIAN_POINT('Ctrl Pts',(8.05403625519527,12.6842105263158,4.64999999999999));
#24919=CARTESIAN_POINT('Ctrl Pts',(6.80807251039055,12.8815789473684,6.80807251039054));
#24920=CARTESIAN_POINT('Ctrl Pts',(4.65,13.078947368421,8.05403625519526));
#24921=CARTESIAN_POINT('Ctrl Pts',(2.49192748960945,13.2763157894737,9.29999999999998));
#24922=CARTESIAN_POINT('Ctrl Pts',(1.99911528227395E-28,13.4736842105263,
9.29999999999999));
#24923=CARTESIAN_POINT('Ctrl Pts',(-2.49192748960944,13.6710526315789,9.29999999999998));
#24924=CARTESIAN_POINT('Ctrl Pts',(-4.64999999999999,13.8684210526316,8.05403625519527));
#24925=CARTESIAN_POINT('Ctrl Pts',(-6.80807251039054,14.0657894736842,6.80807251039054));
#24926=CARTESIAN_POINT('Ctrl Pts',(-8.05403625519527,14.2631578947369,4.64999999999999));
#24927=CARTESIAN_POINT('Ctrl Pts',(-9.29999999999998,14.4605263157895,2.49192748960944));
#24928=CARTESIAN_POINT('Ctrl Pts',(-9.29999999999999,14.6578947368421,5.69460761603425E-16));
#24929=CARTESIAN_POINT('Ctrl Pts',(-9.29999999999998,14.8552631578947,-2.49192748960944));
#24930=CARTESIAN_POINT('Ctrl Pts',(-8.05403625519527,15.0526315789473,-4.64999999999999));
#24931=CARTESIAN_POINT('Ctrl Pts',(-6.80807251039054,15.25,-6.80807251039054));
#24932=CARTESIAN_POINT('Ctrl Pts',(-4.65,15.4473684210526,-8.05403625519526));
#24933=CARTESIAN_POINT('Ctrl Pts',(-2.49192748960944,15.6447368421053,-9.29999999999998));
#24934=CARTESIAN_POINT('Ctrl Pts',(-1.13892152320691E-15,15.8421052631579,
-9.29999999999999));
#24935=CARTESIAN_POINT('Ctrl Pts',(2.49192748960943,16.0394736842105,-9.29999999999999));
#24936=CARTESIAN_POINT('Ctrl Pts',(4.64999999999999,16.2368421052632,-8.05403625519527));
#24937=CARTESIAN_POINT('Ctrl Pts',(6.80807251039054,16.4342105263158,-6.80807251039055));
#24938=CARTESIAN_POINT('Ctrl Pts',(8.05403625519526,16.6315789473684,-4.65));
#24939=CARTESIAN_POINT('Ctrl Pts',(9.29999999999998,16.828947368421,-2.49192748960944));
#24940=CARTESIAN_POINT('Ctrl Pts',(9.29999999999999,17.0263157894737,-1.70838228481055E-15));
#24941=CARTESIAN_POINT('Ctrl Pts',(9.29999999999999,17.2236842105263,2.49192748960943));
#24942=CARTESIAN_POINT('Ctrl Pts',(8.05403625519527,17.4210526315789,4.64999999999998));
#24943=CARTESIAN_POINT('Ctrl Pts',(6.80807251039055,17.6184210526315,6.80807251039054));
#24944=CARTESIAN_POINT('Ctrl Pts',(4.65,17.8157894736842,8.05403625519526));
#24945=CARTESIAN_POINT('Ctrl Pts',(2.49192748960945,18.0131578947368,9.29999999999998));
#24946=CARTESIAN_POINT('Ctrl Pts',(2.5653386859238E-28,18.2105263157895,
9.29999999999999));
#24947=CARTESIAN_POINT('Ctrl Pts',(-2.49192748960944,18.4078947368421,9.29999999999998));
#24948=CARTESIAN_POINT('Ctrl Pts',(-4.64999999999999,18.6052631578947,8.05403625519527));
#24949=CARTESIAN_POINT('Ctrl Pts',(-6.80807251039054,18.8026315789473,6.80807251039054));
#24950=CARTESIAN_POINT('Ctrl Pts',(-8.05403625519527,19.,4.64999999999999));
#24951=CARTESIAN_POINT('Ctrl Pts',(-9.29999999999998,19.1973684210526,2.49192748960944));
#24952=CARTESIAN_POINT('Ctrl Pts',(-9.29999999999999,19.3947368421053,5.69460761603572E-16));
#24953=CARTESIAN_POINT('Ctrl Pts',(-9.29999999999998,19.5921052631579,-2.49192748960944));
#24954=CARTESIAN_POINT('Ctrl Pts',(-8.05403625519527,19.7894736842105,-4.64999999999999));
#24955=CARTESIAN_POINT('Ctrl Pts',(-6.80807251039054,19.9868421052632,-6.80807251039054));
#24956=CARTESIAN_POINT('Ctrl Pts',(-4.65,20.1842105263158,-8.05403625519526));
#24957=CARTESIAN_POINT('Ctrl Pts',(-2.49192748960944,20.3815789473684,-9.29999999999998));
#24958=CARTESIAN_POINT('Ctrl Pts',(-1.13892152320687E-15,20.5789473684211,
-9.29999999999998));
#24959=CARTESIAN_POINT('Ctrl Pts',(2.49192748960943,20.7763157894737,-9.29999999999999));
#24960=CARTESIAN_POINT('Ctrl Pts',(4.64999999999999,20.9736842105263,-8.05403625519526));
#24961=CARTESIAN_POINT('Ctrl Pts',(6.80807251039054,21.171052631579,-6.80807251039055));
#24962=CARTESIAN_POINT('Ctrl Pts',(8.05403625519526,21.3684210526315,-4.65));
#24963=CARTESIAN_POINT('Ctrl Pts',(9.29999999999998,21.5657894736842,-2.49192748960944));
#24964=CARTESIAN_POINT('Ctrl Pts',(9.29999999999999,21.7631578947368,-1.70838228481055E-15));
#24965=CARTESIAN_POINT('Ctrl Pts',(9.29999999999999,21.9605263157895,2.49192748960943));
#24966=CARTESIAN_POINT('Ctrl Pts',(8.05403625519527,22.1578947368421,4.64999999999998));
#24967=CARTESIAN_POINT('Ctrl Pts',(6.80807251039055,22.3552631578947,6.80807251039054));
#24968=CARTESIAN_POINT('Ctrl Pts',(4.65,22.5526315789473,8.05403625519526));
#24969=CARTESIAN_POINT('Ctrl Pts',(2.49192748960945,22.75,9.29999999999998));
#24970=CARTESIAN_POINT('Ctrl Pts',(3.02756187257673E-28,22.9473684210526,
9.29999999999999));
#24971=CARTESIAN_POINT('Ctrl Pts',(-2.49192748960944,23.1447368421053,9.29999999999998));
#24972=CARTESIAN_POINT('Ctrl Pts',(-4.64999999999999,23.3421052631579,8.05403625519527));
#24973=CARTESIAN_POINT('Ctrl Pts',(-6.80807251039054,23.5394736842105,6.80807251039054));
#24974=CARTESIAN_POINT('Ctrl Pts',(-8.05403625519527,23.7368421052632,4.64999999999999));
#24975=CARTESIAN_POINT('Ctrl Pts',(-9.29999999999998,23.9342105263158,2.49192748960944));
#24976=CARTESIAN_POINT('Ctrl Pts',(-9.29999999999999,24.1315789473684,5.69460761603572E-16));
#24977=CARTESIAN_POINT('Ctrl Pts',(-9.29999999999998,24.328947368421,-2.49192748960944));
#24978=CARTESIAN_POINT('Ctrl Pts',(-8.05403625519527,24.5263157894737,-4.64999999999999));
#24979=CARTESIAN_POINT('Ctrl Pts',(-6.80807251039054,24.7236842105264,-6.80807251039054));
#24980=CARTESIAN_POINT('Ctrl Pts',(-4.65,24.921052631579,-8.05403625519526));
#24981=CARTESIAN_POINT('Ctrl Pts',(-2.49192748960944,25.1184210526316,-9.29999999999998));
#24982=CARTESIAN_POINT('Ctrl Pts',(-1.13892152320681E-15,25.3157894736842,
-9.29999999999999));
#24983=CARTESIAN_POINT('Ctrl Pts',(2.49192748960943,25.5131578947368,-9.29999999999999));
#24984=CARTESIAN_POINT('Ctrl Pts',(4.64999999999999,25.7105263157895,-8.05403625519527));
#24985=CARTESIAN_POINT('Ctrl Pts',(6.80807251039054,25.9078947368421,-6.80807251039055));
#24986=CARTESIAN_POINT('Ctrl Pts',(8.05403625519526,26.1052631578947,-4.65));
#24987=CARTESIAN_POINT('Ctrl Pts',(9.29999999999998,26.3026315789474,-2.49192748960944));
#24988=CARTESIAN_POINT('Ctrl Pts',(9.29999999999999,26.5,-1.70838228481055E-15));
#24989=CARTESIAN_POINT('Ctrl Pts',(9.29999999999999,26.6973684210526,2.49192748960943));
#24990=CARTESIAN_POINT('Ctrl Pts',(8.05403625519527,26.8947368421053,4.64999999999998));
#24991=CARTESIAN_POINT('Ctrl Pts',(6.80807251039055,27.0921052631579,6.80807251039054));
#24992=CARTESIAN_POINT('Ctrl Pts',(4.65,27.2894736842105,8.05403625519527));
#24993=CARTESIAN_POINT('Ctrl Pts',(2.49192748960945,27.4868421052631,9.29999999999998));
#24994=CARTESIAN_POINT('Ctrl Pts',(3.53600737789497E-28,27.6842105263158,
9.29999999999999));
#24995=CARTESIAN_POINT('Ctrl Pts',(-2.49192748960944,27.8815789473684,9.29999999999998));
#24996=CARTESIAN_POINT('Ctrl Pts',(-4.64999999999999,28.078947368421,8.05403625519527));
#24997=CARTESIAN_POINT('Ctrl Pts',(-6.80807251039054,28.2763157894736,6.80807251039054));
#24998=CARTESIAN_POINT('Ctrl Pts',(-8.05403625519527,28.4736842105263,4.64999999999999));
#24999=CARTESIAN_POINT('Ctrl Pts',(-9.29999999999998,28.671052631579,2.49192748960944));
#25000=CARTESIAN_POINT('Ctrl Pts',(-9.29999999999999,28.8684210526316,5.69460761603425E-16));
#25001=CARTESIAN_POINT('Ctrl Pts',(-9.29999999999998,29.0657894736842,-2.49192748960944));
#25002=CARTESIAN_POINT('Ctrl Pts',(-8.05403625519527,29.2631578947368,-4.64999999999999));
#25003=CARTESIAN_POINT('Ctrl Pts',(-6.80807251039054,29.4605263157895,-6.80807251039054));
#25004=CARTESIAN_POINT('Ctrl Pts',(-4.65,29.6578947368421,-8.05403625519526));
#25005=CARTESIAN_POINT('Ctrl Pts',(-2.49192748960944,29.8552631578948,-9.29999999999998));
#25006=CARTESIAN_POINT('Ctrl Pts',(-1.13892152320675E-15,30.0526315789474,
-9.29999999999999));
#25007=CARTESIAN_POINT('Ctrl Pts',(2.49192748960943,30.25,-9.29999999999999));
#25008=CARTESIAN_POINT('Ctrl Pts',(4.64999999999999,30.4473684210526,-8.05403625519527));
#25009=CARTESIAN_POINT('Ctrl Pts',(6.80807251039054,30.6447368421053,-6.80807251039055));
#25010=CARTESIAN_POINT('Ctrl Pts',(8.05403625519526,30.8421052631579,-4.65));
#25011=CARTESIAN_POINT('Ctrl Pts',(9.29999999999998,31.0394736842105,-2.49192748960944));
#25012=CARTESIAN_POINT('Ctrl Pts',(9.29999999999999,31.2368421052632,-1.70838228481055E-15));
#25013=CARTESIAN_POINT('Ctrl Pts',(9.29999999999999,31.4342105263158,2.49192748960943));
#25014=CARTESIAN_POINT('Ctrl Pts',(8.05403625519527,31.6315789473684,4.64999999999998));
#25015=CARTESIAN_POINT('Ctrl Pts',(6.80807251039055,31.828947368421,6.80807251039054));
#25016=CARTESIAN_POINT('Ctrl Pts',(4.65,32.0263157894737,8.05403625519526));
#25017=CARTESIAN_POINT('Ctrl Pts',(2.49192748960945,32.2236842105263,9.29999999999998));
#25018=CARTESIAN_POINT('Ctrl Pts',(4.02134172388055E-28,32.421052631579,
9.29999999999999));
#25019=CARTESIAN_POINT('Ctrl Pts',(-2.49192748960944,32.6184210526315,9.29999999999998));
#25020=CARTESIAN_POINT('Ctrl Pts',(-4.64999999999999,32.8157894736842,8.05403625519527));
#25021=CARTESIAN_POINT('Ctrl Pts',(-6.80807251039054,33.0131578947368,6.80807251039054));
#25022=CARTESIAN_POINT('Ctrl Pts',(-8.05403625519527,33.2105263157895,4.64999999999999));
#25023=CARTESIAN_POINT('Ctrl Pts',(-9.29999999999998,33.4078947368421,2.49192748960944));
#25024=CARTESIAN_POINT('Ctrl Pts',(-9.29999999999999,33.6052631578947,5.69460761603425E-16));
#25025=CARTESIAN_POINT('Ctrl Pts',(-9.29999999999998,33.8026315789473,-2.49192748960943));
#25026=CARTESIAN_POINT('Ctrl Pts',(-8.05403625519527,34.,-4.64999999999999));
#25027=CARTESIAN_POINT('Ctrl Pts',(-6.80807251039054,34.1973684210527,-6.80807251039054));
#25028=CARTESIAN_POINT('Ctrl Pts',(-4.65,34.3947368421053,-8.05403625519526));
#25029=CARTESIAN_POINT('Ctrl Pts',(-2.49192748960944,34.5921052631579,-9.29999999999998));
#25030=CARTESIAN_POINT('Ctrl Pts',(-1.13892152320671E-15,34.7894736842105,
-9.29999999999998));
#25031=CARTESIAN_POINT('Ctrl Pts',(2.49192748960943,34.9868421052632,-9.29999999999999));
#25032=CARTESIAN_POINT('Ctrl Pts',(4.64999999999999,35.1842105263158,-8.05403625519526));
#25033=CARTESIAN_POINT('Ctrl Pts',(6.80807251039054,35.3815789473684,-6.80807251039055));
#25034=CARTESIAN_POINT('Ctrl Pts',(8.05403625519526,35.578947368421,-4.65));
#25035=CARTESIAN_POINT('Ctrl Pts',(9.29999999999998,35.7763157894737,-2.49192748960944));
#25036=CARTESIAN_POINT('Ctrl Pts',(9.29999999999999,35.9736842105263,-1.70838228481055E-15));
#25037=CARTESIAN_POINT('Ctrl Pts',(9.29999999999999,36.171052631579,2.49192748960943));
#25038=CARTESIAN_POINT('Ctrl Pts',(8.05403625519527,36.3684210526316,4.64999999999999));
#25039=CARTESIAN_POINT('Ctrl Pts',(6.80807251039055,36.5657894736842,6.80807251039054));
#25040=CARTESIAN_POINT('Ctrl Pts',(4.65,36.7631578947368,8.05403625519526));
#25041=CARTESIAN_POINT('Ctrl Pts',(2.49192748960945,36.9605263157895,9.29999999999998));
#25042=CARTESIAN_POINT('Ctrl Pts',(4.63378744619569E-28,37.1578947368421,
9.29999999999999));
#25043=CARTESIAN_POINT('Ctrl Pts',(-2.49192748960944,37.3552631578947,9.29999999999998));
#25044=CARTESIAN_POINT('Ctrl Pts',(-4.64999999999999,37.5526315789473,8.05403625519527));
#25045=CARTESIAN_POINT('Ctrl Pts',(-6.80807251039054,37.7499999999999,6.80807251039054));
#25046=CARTESIAN_POINT('Ctrl Pts',(-8.05403625519527,37.9473684210526,4.64999999999999));
#25047=CARTESIAN_POINT('Ctrl Pts',(-9.29999999999998,38.1447368421053,2.49192748960944));
#25048=CARTESIAN_POINT('Ctrl Pts',(-9.29999999999999,38.3421052631579,5.69460761603425E-16));
#25049=CARTESIAN_POINT('Ctrl Pts',(-9.29999999999998,38.5394736842105,-2.49192748960943));
#25050=CARTESIAN_POINT('Ctrl Pts',(-8.05403625519527,38.7368421052631,-4.64999999999999));
#25051=CARTESIAN_POINT('Ctrl Pts',(-6.80807251039054,38.9342105263158,-6.80807251039054));
#25052=CARTESIAN_POINT('Ctrl Pts',(-4.65,39.1315789473684,-8.05403625519526));
#25053=CARTESIAN_POINT('Ctrl Pts',(-2.49192748960944,39.328947368421,-9.29999999999998));
#25054=CARTESIAN_POINT('Ctrl Pts',(-1.13892152320665E-15,39.5263157894737,
-9.29999999999999));
#25055=CARTESIAN_POINT('Ctrl Pts',(2.49192748960943,39.7236842105263,-9.29999999999999));
#25056=CARTESIAN_POINT('Ctrl Pts',(4.64999999999999,39.921052631579,-8.05403625519527));
#25057=CARTESIAN_POINT('Ctrl Pts',(6.80807251039054,40.1184210526316,-6.80807251039055));
#25058=CARTESIAN_POINT('Ctrl Pts',(8.05403625519526,40.3157894736842,-4.65));
#25059=CARTESIAN_POINT('Ctrl Pts',(9.29999999999998,40.5131578947368,-2.49192748960944));
#25060=CARTESIAN_POINT('Ctrl Pts',(9.29999999999999,40.7105263157895,-1.70838228481055E-15));
#25061=CARTESIAN_POINT('Ctrl Pts',(9.29999999999999,40.9078947368421,2.49192748960943));
#25062=CARTESIAN_POINT('Ctrl Pts',(8.05403625519527,41.1052631578948,4.64999999999998));
#25063=CARTESIAN_POINT('Ctrl Pts',(6.80807251039055,41.3026315789473,6.80807251039054));
#25064=CARTESIAN_POINT('Ctrl Pts',(4.65,41.5,8.05403625519527));
#25065=CARTESIAN_POINT('Ctrl Pts',(2.49192748960945,41.6973684210526,9.29999999999998));
#25066=CARTESIAN_POINT('Ctrl Pts',(5.1306773718476E-28,41.8947368421053,
9.29999999999999));
#25067=CARTESIAN_POINT('Ctrl Pts',(-2.49192748960944,42.0921052631579,9.29999999999998));
#25068=CARTESIAN_POINT('Ctrl Pts',(-4.64999999999999,42.2894736842105,8.05403625519527));
#25069=CARTESIAN_POINT('Ctrl Pts',(-6.80807251039054,42.4868421052631,6.80807251039054));
#25070=CARTESIAN_POINT('Ctrl Pts',(-8.05403625519527,42.6842105263158,4.64999999999999));
#25071=CARTESIAN_POINT('Ctrl Pts',(-9.29999999999998,42.8815789473684,2.49192748960944));
#25072=CARTESIAN_POINT('Ctrl Pts',(-9.29999999999999,43.078947368421,5.69460761603425E-16));
#25073=CARTESIAN_POINT('Ctrl Pts',(-9.29999999999998,43.2763157894737,-2.49192748960943));
#25074=CARTESIAN_POINT('Ctrl Pts',(-8.05403625519527,43.4736842105263,-4.64999999999999));
#25075=CARTESIAN_POINT('Ctrl Pts',(-6.80807251039054,43.671052631579,-6.80807251039054));
#25076=CARTESIAN_POINT('Ctrl Pts',(-4.65,43.8684210526316,-8.05403625519526));
#25077=CARTESIAN_POINT('Ctrl Pts',(-2.49192748960944,44.0657894736842,-9.29999999999998));
#25078=CARTESIAN_POINT('Ctrl Pts',(-1.13892152320661E-15,44.2631578947368,
-9.29999999999999));
#25079=CARTESIAN_POINT('Ctrl Pts',(2.49192748960943,44.4605263157895,-9.29999999999999));
#25080=CARTESIAN_POINT('Ctrl Pts',(4.64999999999999,44.6578947368421,-8.05403625519527));
#25081=CARTESIAN_POINT('Ctrl Pts',(6.80807251039054,44.8552631578948,-6.80807251039055));
#25082=CARTESIAN_POINT('Ctrl Pts',(8.05403625519526,45.0526315789473,-4.65));
#25083=CARTESIAN_POINT('Ctrl Pts',(9.29999999999998,45.25,-2.49192748960945));
#25084=CARTESIAN_POINT('Ctrl Pts',(9.29999999999999,45.4473684210526,-1.70838228481055E-15));
#25085=CARTESIAN_POINT('Ctrl Pts',(9.29999999999999,45.6447368421053,2.49192748960943));
#25086=CARTESIAN_POINT('Ctrl Pts',(8.05403625519527,45.8421052631579,4.64999999999999));
#25087=CARTESIAN_POINT('Ctrl Pts',(6.80807251039055,46.0394736842105,6.80807251039054));
#25088=CARTESIAN_POINT('Ctrl Pts',(4.65,46.2368421052631,8.05403625519526));
#25089=CARTESIAN_POINT('Ctrl Pts',(2.49192748960945,46.4342105263158,9.29999999999998));
#25090=CARTESIAN_POINT('Ctrl Pts',(5.61601171783318E-28,46.6315789473684,
9.29999999999999));
#25091=CARTESIAN_POINT('Ctrl Pts',(-2.49192748960944,46.828947368421,9.29999999999998));
#25092=CARTESIAN_POINT('Ctrl Pts',(-4.64999999999999,47.0263157894737,8.05403625519527));
#25093=CARTESIAN_POINT('Ctrl Pts',(-6.80807251039054,47.2236842105263,6.80807251039054));
#25094=CARTESIAN_POINT('Ctrl Pts',(-8.05403625519527,47.421052631579,4.64999999999999));
#25095=CARTESIAN_POINT('Ctrl Pts',(-9.29999999999998,47.6184210526316,2.49192748960944));
#25096=CARTESIAN_POINT('Ctrl Pts',(-9.29999999999999,47.8157894736842,5.69460761603572E-16));
#25097=CARTESIAN_POINT('Ctrl Pts',(-9.29999999999998,48.0131578947368,-2.49192748960943));
#25098=CARTESIAN_POINT('Ctrl Pts',(-8.05403625519527,48.2105263157894,-4.64999999999999));
#25099=CARTESIAN_POINT('Ctrl Pts',(-6.80807251039054,48.4078947368421,-6.80807251039054));
#25100=CARTESIAN_POINT('Ctrl Pts',(-4.65,48.6052631578947,-8.05403625519526));
#25101=CARTESIAN_POINT('Ctrl Pts',(-2.49192748960944,48.8026315789474,-9.29999999999998));
#25102=CARTESIAN_POINT('Ctrl Pts',(-1.13892152320655E-15,49.,-9.29999999999998));
#25103=CARTESIAN_POINT('Ctrl Pts',(2.49192748960943,49.1973684210527,-9.29999999999999));
#25104=CARTESIAN_POINT('Ctrl Pts',(4.64999999999999,49.3947368421053,-8.05403625519527));
#25105=CARTESIAN_POINT('Ctrl Pts',(6.80807251039054,49.5921052631579,-6.80807251039055));
#25106=CARTESIAN_POINT('Ctrl Pts',(8.05403625519526,49.7894736842104,-4.65));
#25107=CARTESIAN_POINT('Ctrl Pts',(9.29999999999998,49.9868421052631,-2.49192748960945));
#25108=CARTESIAN_POINT('Ctrl Pts',(9.29999999999999,50.1842105263158,-1.70838228481055E-15));
#25109=CARTESIAN_POINT('Ctrl Pts',(9.29999999999999,50.3815789473684,2.49192748960943));
#25110=CARTESIAN_POINT('Ctrl Pts',(8.05403625519527,50.5789473684211,4.64999999999998));
#25111=CARTESIAN_POINT('Ctrl Pts',(6.80807251039055,50.7763157894736,6.80807251039054));
#25112=CARTESIAN_POINT('Ctrl Pts',(4.65,50.9736842105263,8.05403625519526));
#25113=CARTESIAN_POINT('Ctrl Pts',(2.49192748960945,51.1710526315789,9.29999999999998));
#25114=CARTESIAN_POINT('Ctrl Pts',(6.1706795418167E-28,51.3684210526316,
9.29999999999999));
#25115=CARTESIAN_POINT('Ctrl Pts',(-2.49192748960944,51.5657894736842,9.29999999999998));
#25116=CARTESIAN_POINT('Ctrl Pts',(-4.64999999999999,51.7631578947368,8.05403625519527));
#25117=CARTESIAN_POINT('Ctrl Pts',(-6.80807251039054,51.9605263157894,6.80807251039054));
#25118=CARTESIAN_POINT('Ctrl Pts',(-8.05403625519527,52.1578947368421,4.64999999999999));
#25119=CARTESIAN_POINT('Ctrl Pts',(-9.29999999999998,52.3552631578947,2.49192748960944));
#25120=CARTESIAN_POINT('Ctrl Pts',(-9.29999999999999,52.5526315789474,5.69460761603572E-16));
#25121=CARTESIAN_POINT('Ctrl Pts',(-9.29999999999998,52.75,-2.49192748960944));
#25122=CARTESIAN_POINT('Ctrl Pts',(-8.05403625519527,52.9473684210526,-4.64999999999999));
#25123=CARTESIAN_POINT('Ctrl Pts',(-6.80807251039054,53.1447368421053,-6.80807251039054));
#25124=CARTESIAN_POINT('Ctrl Pts',(-4.65,53.3421052631579,-8.05403625519526));
#25125=CARTESIAN_POINT('Ctrl Pts',(-2.49192748960944,53.5394736842105,-9.29999999999998));
#25126=CARTESIAN_POINT('Ctrl Pts',(-1.1389215232065E-15,53.7368421052632,
-9.29999999999999));
#25127=CARTESIAN_POINT('Ctrl Pts',(2.49192748960943,53.9342105263158,-9.29999999999999));
#25128=CARTESIAN_POINT('Ctrl Pts',(4.64999999999999,54.1315789473684,-8.05403625519526));
#25129=CARTESIAN_POINT('Ctrl Pts',(6.80807251039054,54.3289473684211,-6.80807251039055));
#25130=CARTESIAN_POINT('Ctrl Pts',(8.05403625519526,54.5263157894736,-4.65));
#25131=CARTESIAN_POINT('Ctrl Pts',(9.29999999999998,54.7236842105263,-2.49192748960944));
#25132=CARTESIAN_POINT('Ctrl Pts',(9.29999999999999,54.9210526315789,-1.7083822848104E-15));
#25133=CARTESIAN_POINT('Ctrl Pts',(9.29999999999999,55.1184210526316,2.49192748960943));
#25134=CARTESIAN_POINT('Ctrl Pts',(8.05403625519527,55.3157894736842,4.64999999999998));
#25135=CARTESIAN_POINT('Ctrl Pts',(6.80807251039055,55.5131578947368,6.80807251039054));
#25136=CARTESIAN_POINT('Ctrl Pts',(4.65,55.7105263157895,8.05403625519526));
#25137=CARTESIAN_POINT('Ctrl Pts',(2.49192748960945,55.9078947368421,9.29999999999998));
#25138=CARTESIAN_POINT('Ctrl Pts',(6.59823598947067E-28,56.1052631578947,
9.29999999999999));
#25139=CARTESIAN_POINT('Ctrl Pts',(-2.49192748960944,56.3026315789474,9.29999999999998));
#25140=CARTESIAN_POINT('Ctrl Pts',(-4.64999999999999,56.5,8.05403625519527));
#25141=CARTESIAN_POINT('Ctrl Pts',(-6.80807251039054,56.6973684210526,6.80807251039054));
#25142=CARTESIAN_POINT('Ctrl Pts',(-8.05403625519527,56.8947368421053,4.64999999999999));
#25143=CARTESIAN_POINT('Ctrl Pts',(-9.29999999999998,57.0921052631579,2.49192748960944));
#25144=CARTESIAN_POINT('Ctrl Pts',(-9.29999999999999,57.2894736842105,5.69460761603572E-16));
#25145=CARTESIAN_POINT('Ctrl Pts',(-9.29999999999998,57.4868421052631,-2.49192748960944));
#25146=CARTESIAN_POINT('Ctrl Pts',(-8.05403625519527,57.6842105263157,-4.64999999999999));
#25147=CARTESIAN_POINT('Ctrl Pts',(-6.80807251039054,57.8815789473684,-6.80807251039054));
#25148=CARTESIAN_POINT('Ctrl Pts',(-4.65,58.0789473684211,-8.05403625519526));
#25149=CARTESIAN_POINT('Ctrl Pts',(-2.49192748960944,58.2763157894737,-9.29999999999998));
#25150=CARTESIAN_POINT('Ctrl Pts',(-1.13892152320645E-15,58.4736842105264,
-9.29999999999999));
#25151=CARTESIAN_POINT('Ctrl Pts',(2.49192748960943,58.671052631579,-9.29999999999999));
#25152=CARTESIAN_POINT('Ctrl Pts',(4.64999999999999,58.8684210526316,-8.05403625519527));
#25153=CARTESIAN_POINT('Ctrl Pts',(6.80807251039054,59.0657894736842,-6.80807251039055));
#25154=CARTESIAN_POINT('Ctrl Pts',(8.05403625519526,59.2631578947368,-4.65));
#25155=CARTESIAN_POINT('Ctrl Pts',(9.29999999999998,59.4605263157895,-2.49192748960944));
#25156=CARTESIAN_POINT('Ctrl Pts',(9.29999999999999,59.6578947368421,-1.7083822848104E-15));
#25157=CARTESIAN_POINT('Ctrl Pts',(9.29999999999999,59.8552631578947,2.49192748960943));
#25158=CARTESIAN_POINT('Ctrl Pts',(8.05403625519527,60.0526315789474,4.64999999999999));
#25159=CARTESIAN_POINT('Ctrl Pts',(6.80807251039055,60.25,6.80807251039054));
#25160=CARTESIAN_POINT('Ctrl Pts',(4.65,60.4473684210526,8.05403625519526));
#25161=CARTESIAN_POINT('Ctrl Pts',(2.49192748960945,60.6447368421052,9.29999999999998));
#25162=CARTESIAN_POINT('Ctrl Pts',(7.18757055245316E-28,60.8421052631579,
9.29999999999999));
#25163=CARTESIAN_POINT('Ctrl Pts',(-2.49192748960944,61.0394736842105,9.29999999999998));
#25164=CARTESIAN_POINT('Ctrl Pts',(-4.64999999999999,61.2368421052631,8.05403625519527));
#25165=CARTESIAN_POINT('Ctrl Pts',(-6.80807251039054,61.4342105263157,6.80807251039054));
#25166=CARTESIAN_POINT('Ctrl Pts',(-8.05403625519527,61.6315789473685,4.64999999999999));
#25167=CARTESIAN_POINT('Ctrl Pts',(-9.29999999999998,61.8289473684211,2.49192748960944));
#25168=CARTESIAN_POINT('Ctrl Pts',(-9.29999999999999,62.0263157894737,5.69460761603425E-16));
#25169=CARTESIAN_POINT('Ctrl Pts',(-9.29999999999998,62.2236842105263,-2.49192748960944));
#25170=CARTESIAN_POINT('Ctrl Pts',(-8.05403625519527,62.4210526315789,-4.64999999999999));
#25171=CARTESIAN_POINT('Ctrl Pts',(-6.80807251039054,62.6184210526316,-6.80807251039054));
#25172=CARTESIAN_POINT('Ctrl Pts',(-4.65,62.8157894736842,-8.05403625519526));
#25173=CARTESIAN_POINT('Ctrl Pts',(-2.49192748960944,63.0131578947368,-9.29999999999998));
#25174=CARTESIAN_POINT('Ctrl Pts',(-1.13892152320639E-15,63.2105263157895,
-9.29999999999999));
#25175=CARTESIAN_POINT('Ctrl Pts',(2.49192748960943,63.4078947368421,-9.29999999999999));
#25176=CARTESIAN_POINT('Ctrl Pts',(4.64999999999999,63.6052631578947,-8.05403625519527));
#25177=CARTESIAN_POINT('Ctrl Pts',(6.80807251039054,63.8026315789474,-6.80807251039055));
#25178=CARTESIAN_POINT('Ctrl Pts',(8.05403625519526,64.,-4.65));
#25179=CARTESIAN_POINT('Ctrl Pts',(9.29999999999998,64.1973684210526,-2.49192748960944));
#25180=CARTESIAN_POINT('Ctrl Pts',(9.29999999999999,64.3947368421052,-1.7083822848104E-15));
#25181=CARTESIAN_POINT('Ctrl Pts',(9.29999999999999,64.5921052631579,2.49192748960943));
#25182=CARTESIAN_POINT('Ctrl Pts',(8.05403625519527,64.7894736842105,4.64999999999998));
#25183=CARTESIAN_POINT('Ctrl Pts',(6.80807251039055,64.9868421052631,6.80807251039053));
#25184=CARTESIAN_POINT('Ctrl Pts',(4.65,65.1842105263158,8.05403625519526));
#25185=CARTESIAN_POINT('Ctrl Pts',(2.49192748960945,65.3815789473684,9.29999999999998));
#25186=CARTESIAN_POINT('Ctrl Pts',(7.69601605777139E-28,65.578947368421,
9.29999999999999));
#25187=CARTESIAN_POINT('Ctrl Pts',(-2.49192748960944,65.7763157894737,9.29999999999999));
#25188=CARTESIAN_POINT('Ctrl Pts',(-4.64999999999999,65.9736842105263,8.05403625519527));
#25189=CARTESIAN_POINT('Ctrl Pts',(-6.80807251039054,66.1710526315789,6.80807251039055));
#25190=CARTESIAN_POINT('Ctrl Pts',(-8.05403625519527,66.3684210526316,4.64999999999999));
#25191=CARTESIAN_POINT('Ctrl Pts',(-9.29999999999998,66.5657894736842,2.49192748960944));
#25192=CARTESIAN_POINT('Ctrl Pts',(-9.29999999999999,66.7631578947368,5.69460761603572E-16));
#25193=CARTESIAN_POINT('Ctrl Pts',(-9.29999999999998,66.9605263157895,-2.49192748960944));
#25194=CARTESIAN_POINT('Ctrl Pts',(-8.05403625519527,67.1578947368421,-4.64999999999999));
#25195=CARTESIAN_POINT('Ctrl Pts',(-6.80807251039054,67.3552631578948,-6.80807251039054));
#25196=CARTESIAN_POINT('Ctrl Pts',(-4.65,67.5526315789474,-8.05403625519526));
#25197=CARTESIAN_POINT('Ctrl Pts',(-2.49192748960944,67.75,-9.29999999999998));
#25198=CARTESIAN_POINT('Ctrl Pts',(-1.13892152320635E-15,67.9473684210527,
-9.29999999999998));
#25199=CARTESIAN_POINT('Ctrl Pts',(2.49192748960943,68.1447368421053,-9.29999999999999));
#25200=CARTESIAN_POINT('Ctrl Pts',(4.64999999999999,68.3421052631579,-8.05403625519526));
#25201=CARTESIAN_POINT('Ctrl Pts',(6.80807251039054,68.5394736842105,-6.80807251039055));
#25202=CARTESIAN_POINT('Ctrl Pts',(8.05403625519526,68.7368421052631,-4.65));
#25203=CARTESIAN_POINT('Ctrl Pts',(9.29999999999998,68.9342105263158,-2.49192748960944));
#25204=CARTESIAN_POINT('Ctrl Pts',(9.29999999999999,69.1315789473684,-1.7083822848104E-15));
#25205=CARTESIAN_POINT('Ctrl Pts',(9.29999999999999,69.3289473684211,2.49192748960943));
#25206=CARTESIAN_POINT('Ctrl Pts',(8.05403625519527,69.5263157894737,4.64999999999999));
#25207=CARTESIAN_POINT('Ctrl Pts',(6.80807251039055,69.7236842105263,6.80807251039054));
#25208=CARTESIAN_POINT('Ctrl Pts',(4.65,69.9210526315789,8.05403625519526));
#25209=CARTESIAN_POINT('Ctrl Pts',(2.49192748960945,70.1184210526316,9.29999999999998));
#25210=CARTESIAN_POINT('Ctrl Pts',(8.22757272242227E-28,70.3157894736842,
9.29999999999999));
#25211=CARTESIAN_POINT('Ctrl Pts',(-2.49192748960944,70.5131578947368,9.29999999999998));
#25212=CARTESIAN_POINT('Ctrl Pts',(-4.64999999999999,70.7105263157894,8.05403625519527));
#25213=CARTESIAN_POINT('Ctrl Pts',(-6.80807251039054,70.9078947368421,6.80807251039054));
#25214=CARTESIAN_POINT('Ctrl Pts',(-8.05403625519527,71.1052631578948,4.64999999999999));
#25215=CARTESIAN_POINT('Ctrl Pts',(-9.29999999999998,71.3026315789474,2.49192748960944));
#25216=CARTESIAN_POINT('Ctrl Pts',(-9.29999999999999,71.5,5.69460761603572E-16));
#25217=CARTESIAN_POINT('Ctrl Pts',(-9.29999999999998,71.6973684210526,-2.49192748960943));
#25218=CARTESIAN_POINT('Ctrl Pts',(-8.05403625519527,71.8947368421052,-4.64999999999999));
#25219=CARTESIAN_POINT('Ctrl Pts',(-6.80807251039054,72.0921052631579,-6.80807251039054));
#25220=CARTESIAN_POINT('Ctrl Pts',(-4.65,72.2894736842105,-8.05403625519526));
#25221=CARTESIAN_POINT('Ctrl Pts',(-2.49192748960944,72.4868421052632,-9.29999999999998));
#25222=CARTESIAN_POINT('Ctrl Pts',(-1.13892152320629E-15,72.6842105263158,
-9.29999999999999));
#25223=CARTESIAN_POINT('Ctrl Pts',(2.49192748960943,72.8815789473684,-9.29999999999999));
#25224=CARTESIAN_POINT('Ctrl Pts',(4.64999999999999,73.078947368421,-8.05403625519527));
#25225=CARTESIAN_POINT('Ctrl Pts',(6.80807251039054,73.2763157894738,-6.80807251039055));
#25226=CARTESIAN_POINT('Ctrl Pts',(8.05403625519526,73.4736842105262,-4.65));
#25227=CARTESIAN_POINT('Ctrl Pts',(9.29999999999998,73.6710526315789,-2.49192748960944));
#25228=CARTESIAN_POINT('Ctrl Pts',(9.29999999999999,73.8684210526316,-1.7083822848104E-15));
#25229=CARTESIAN_POINT('Ctrl Pts',(9.29999999999999,74.0657894736842,2.49192748960943));
#25230=CARTESIAN_POINT('Ctrl Pts',(8.05403625519527,74.2631578947368,4.64999999999998));
#25231=CARTESIAN_POINT('Ctrl Pts',(6.80807251039055,74.4605263157894,6.80807251039054));
#25232=CARTESIAN_POINT('Ctrl Pts',(4.65,74.6578947368421,8.05403625519527));
#25233=CARTESIAN_POINT('Ctrl Pts',(2.49192748960945,74.8552631578947,9.29999999999998));
#25234=CARTESIAN_POINT('Ctrl Pts',(8.7360182277405E-28,75.0526315789473,
9.29999999999999));
#25235=CARTESIAN_POINT('Ctrl Pts',(-2.49192748960944,75.25,9.29999999999998));
#25236=CARTESIAN_POINT('Ctrl Pts',(-4.64999999999999,75.4473684210526,8.05403625519527));
#25237=CARTESIAN_POINT('Ctrl Pts',(-6.80807251039054,75.6447368421052,6.80807251039054));
#25238=CARTESIAN_POINT('Ctrl Pts',(-8.05403625519527,75.8421052631579,4.64999999999999));
#25239=CARTESIAN_POINT('Ctrl Pts',(-9.29999999999998,76.0394736842105,2.49192748960944));
#25240=CARTESIAN_POINT('Ctrl Pts',(-9.29999999999999,76.2368421052631,5.69460761603572E-16));
#25241=CARTESIAN_POINT('Ctrl Pts',(-9.29999999999998,76.4342105263158,-2.49192748960943));
#25242=CARTESIAN_POINT('Ctrl Pts',(-8.05403625519527,76.6315789473684,-4.64999999999999));
#25243=CARTESIAN_POINT('Ctrl Pts',(-6.80807251039054,76.8289473684211,-6.80807251039054));
#25244=CARTESIAN_POINT('Ctrl Pts',(-4.65,77.0263157894737,-8.05403625519526));
#25245=CARTESIAN_POINT('Ctrl Pts',(-2.49192748960944,77.2236842105263,-9.29999999999998));
#25246=CARTESIAN_POINT('Ctrl Pts',(-1.13892152320624E-15,77.4210526315789,
-9.29999999999999));
#25247=CARTESIAN_POINT('Ctrl Pts',(2.49192748960943,77.6184210526316,-9.29999999999999));
#25248=CARTESIAN_POINT('Ctrl Pts',(4.64999999999999,77.8157894736842,-8.05403625519527));
#25249=CARTESIAN_POINT('Ctrl Pts',(6.80807251039054,78.0131578947369,-6.80807251039055));
#25250=CARTESIAN_POINT('Ctrl Pts',(8.05403625519526,78.2105263157894,-4.65));
#25251=CARTESIAN_POINT('Ctrl Pts',(9.29999999999998,78.4078947368421,-2.49192748960944));
#25252=CARTESIAN_POINT('Ctrl Pts',(9.29999999999999,78.6052631578947,-1.70838228481055E-15));
#25253=CARTESIAN_POINT('Ctrl Pts',(9.29999999999999,78.8026315789474,2.49192748960943));
#25254=CARTESIAN_POINT('Ctrl Pts',(8.05403625519527,79.,4.64999999999999));
#25255=CARTESIAN_POINT('Ctrl Pts',(6.80807251039055,79.1973684210526,6.80807251039054));
#25256=CARTESIAN_POINT('Ctrl Pts',(4.65,79.3947368421052,8.05403625519526));
#25257=CARTESIAN_POINT('Ctrl Pts',(2.49192748960945,79.5921052631579,9.29999999999998));
#25258=CARTESIAN_POINT('Ctrl Pts',(9.22135257372608E-28,79.7894736842105,
9.29999999999999));
#25259=CARTESIAN_POINT('Ctrl Pts',(-2.49192748960944,79.9868421052632,9.29999999999998));
#25260=CARTESIAN_POINT('Ctrl Pts',(-4.64999999999999,80.1842105263158,8.05403625519527));
#25261=CARTESIAN_POINT('Ctrl Pts',(-6.80807251039054,80.3815789473684,6.80807251039054));
#25262=CARTESIAN_POINT('Ctrl Pts',(-8.05403625519527,80.5789473684211,4.64999999999999));
#25263=CARTESIAN_POINT('Ctrl Pts',(-9.29999999999998,80.7763157894737,2.49192748960944));
#25264=CARTESIAN_POINT('Ctrl Pts',(-9.29999999999999,80.9736842105263,5.69460761603572E-16));
#25265=CARTESIAN_POINT('Ctrl Pts',(-9.29999999999998,81.1710526315789,-2.49192748960943));
#25266=CARTESIAN_POINT('Ctrl Pts',(-8.05403625519527,81.3684210526315,-4.64999999999999));
#25267=CARTESIAN_POINT('Ctrl Pts',(-6.80807251039054,81.5657894736842,-6.80807251039054));
#25268=CARTESIAN_POINT('Ctrl Pts',(-4.65,81.7631578947368,-8.05403625519526));
#25269=CARTESIAN_POINT('Ctrl Pts',(-2.49192748960944,81.9605263157895,-9.29999999999998));
#25270=CARTESIAN_POINT('Ctrl Pts',(-1.13892152320619E-15,82.1578947368421,
-9.29999999999998));
#25271=CARTESIAN_POINT('Ctrl Pts',(2.49192748960943,82.3552631578947,-9.29999999999999));
#25272=CARTESIAN_POINT('Ctrl Pts',(4.64999999999999,82.5526315789474,-8.05403625519527));
#25273=CARTESIAN_POINT('Ctrl Pts',(6.80807251039054,82.7500000000001,-6.80807251039055));
#25274=CARTESIAN_POINT('Ctrl Pts',(8.05403625519526,82.9473684210525,-4.65));
#25275=CARTESIAN_POINT('Ctrl Pts',(9.29999999999998,83.1447368421052,-2.49192748960944));
#25276=CARTESIAN_POINT('Ctrl Pts',(9.29999999999999,83.3421052631579,-1.70838228481055E-15));
#25277=CARTESIAN_POINT('Ctrl Pts',(9.29999999999999,83.5394736842105,2.49192748960943));
#25278=CARTESIAN_POINT('Ctrl Pts',(8.05403625519527,83.7368421052632,4.64999999999998));
#25279=CARTESIAN_POINT('Ctrl Pts',(6.80807251039055,83.9342105263157,6.80807251039054));
#25280=CARTESIAN_POINT('Ctrl Pts',(4.65,84.1315789473684,8.05403625519526));
#25281=CARTESIAN_POINT('Ctrl Pts',(2.49192748960945,84.328947368421,9.29999999999998));
#25282=CARTESIAN_POINT('Ctrl Pts',(9.8222427163749E-28,84.5263157894737,
9.29999999999999));
#25283=CARTESIAN_POINT('Ctrl Pts',(-2.49192748960944,84.7236842105263,9.29999999999998));
#25284=CARTESIAN_POINT('Ctrl Pts',(-4.64999999999999,84.9210526315789,8.05403625519527));
#25285=CARTESIAN_POINT('Ctrl Pts',(-6.80807251039054,85.1184210526315,6.80807251039054));
#25286=CARTESIAN_POINT('Ctrl Pts',(-8.05403625519527,85.3157894736842,4.64999999999999));
#25287=CARTESIAN_POINT('Ctrl Pts',(-9.29999999999998,85.5131578947368,2.49192748960944));
#25288=CARTESIAN_POINT('Ctrl Pts',(-9.29999999999999,85.7105263157894,5.69460761603425E-16));
#25289=CARTESIAN_POINT('Ctrl Pts',(-9.29999999999998,85.9078947368421,-2.49192748960943));
#25290=CARTESIAN_POINT('Ctrl Pts',(-8.05403625519527,86.1052631578947,-4.64999999999999));
#25291=CARTESIAN_POINT('Ctrl Pts',(-6.80807251039054,86.3026315789474,-6.80807251039054));
#25292=CARTESIAN_POINT('Ctrl Pts',(-4.65,86.5,-8.05403625519526));
#25293=CARTESIAN_POINT('Ctrl Pts',(-2.49192748960944,86.6973684210526,-9.29999999999998));
#25294=CARTESIAN_POINT('Ctrl Pts',(-1.13892152320614E-15,86.8947368421052,
-9.29999999999999));
#25295=CARTESIAN_POINT('Ctrl Pts',(2.49192748960943,87.0921052631579,-9.29999999999999));
#25296=CARTESIAN_POINT('Ctrl Pts',(4.64999999999999,87.2894736842105,-8.05403625519526));
#25297=CARTESIAN_POINT('Ctrl Pts',(6.80807251039054,87.4868421052632,-6.80807251039055));
#25298=CARTESIAN_POINT('Ctrl Pts',(8.05403625519526,87.6842105263158,-4.65));
#25299=CARTESIAN_POINT('Ctrl Pts',(9.29999999999998,87.8815789473684,-2.49192748960945));
#25300=CARTESIAN_POINT('Ctrl Pts',(9.29999999999999,88.078947368421,-1.7083822848107E-15));
#25301=CARTESIAN_POINT('Ctrl Pts',(9.29999999999999,88.2763157894737,2.49192748960943));
#25302=CARTESIAN_POINT('Ctrl Pts',(8.05403625519527,88.4736842105263,4.64999999999998));
#25303=CARTESIAN_POINT('Ctrl Pts',(6.80807251039055,88.6710526315789,6.80807251039054));
#25304=CARTESIAN_POINT('Ctrl Pts',(4.65,88.8684210526316,8.05403625519526));
#25305=CARTESIAN_POINT('Ctrl Pts',(2.49192748960945,89.0657894736842,9.29999999999998));
#25306=CARTESIAN_POINT('Ctrl Pts',(1.02613547436952E-27,89.2631578947368,
9.29999999999999));
#25307=CARTESIAN_POINT('Ctrl Pts',(-2.49192748960944,89.4605263157895,9.29999999999998));
#25308=CARTESIAN_POINT('Ctrl Pts',(-4.64999999999999,89.6578947368421,8.05403625519527));
#25309=CARTESIAN_POINT('Ctrl Pts',(-6.80807251039054,89.8552631578947,6.80807251039054));
#25310=CARTESIAN_POINT('Ctrl Pts',(-8.05403625519527,90.0526315789474,4.64999999999999));
#25311=CARTESIAN_POINT('Ctrl Pts',(-9.29999999999998,90.25,2.49192748960944));
#25312=CARTESIAN_POINT('Ctrl Pts',(-9.29999999999999,90.4473684210526,5.69460761603572E-16));
#25313=CARTESIAN_POINT('Ctrl Pts',(-9.29999999999998,90.6447368421053,-2.49192748960943));
#25314=CARTESIAN_POINT('Ctrl Pts',(-8.05403625519527,90.8421052631578,-4.64999999999999));
#25315=CARTESIAN_POINT('Ctrl Pts',(-6.80807251039054,91.0394736842106,-6.80807251039054));
#25316=CARTESIAN_POINT('Ctrl Pts',(-4.65,91.2368421052632,-8.05403625519526));
#25317=CARTESIAN_POINT('Ctrl Pts',(-2.49192748960944,91.4342105263158,-9.29999999999998));
#25318=CARTESIAN_POINT('Ctrl Pts',(-1.13892152320609E-15,91.6315789473685,
-9.29999999999999));
#25319=CARTESIAN_POINT('Ctrl Pts',(2.49192748960943,91.828947368421,-9.29999999999999));
#25320=CARTESIAN_POINT('Ctrl Pts',(4.64999999999999,92.0263157894737,-8.05403625519527));
#25321=CARTESIAN_POINT('Ctrl Pts',(6.80807251039054,92.2236842105264,-6.80807251039055));
#25322=CARTESIAN_POINT('Ctrl Pts',(8.05403625519526,92.4210526315789,-4.65));
#25323=CARTESIAN_POINT('Ctrl Pts',(9.29999999999998,92.6184210526316,-2.49192748960945));
#25324=CARTESIAN_POINT('Ctrl Pts',(9.29999999999999,92.8157894736842,-1.70838228481055E-15));
#25325=CARTESIAN_POINT('Ctrl Pts',(9.29999999999999,93.0131578947368,2.49192748960943));
#25326=CARTESIAN_POINT('Ctrl Pts',(8.05403625519527,93.2105263157895,4.64999999999999));
#25327=CARTESIAN_POINT('Ctrl Pts',(6.80807251039055,93.4078947368421,6.80807251039054));
#25328=CARTESIAN_POINT('Ctrl Pts',(4.65,93.6052631578947,8.05403625519526));
#25329=CARTESIAN_POINT('Ctrl Pts',(2.49192748960945,93.8026315789474,9.29999999999998));
#25330=CARTESIAN_POINT('Ctrl Pts',(1.08160225676787E-27,94.,9.29999999999999));
#25331=CARTESIAN_POINT('Ctrl Pts',(5.54667823983524E-29,0.,9.29999999999998));
#25332=CARTESIAN_POINT('Ctrl Pts',(-2.49192748960943,0.197368421052581,
9.29999999999998));
#25333=CARTESIAN_POINT('Ctrl Pts',(-4.64999999999999,0.394736842105226,
8.05403625519526));
#25334=CARTESIAN_POINT('Ctrl Pts',(-6.80807251039055,0.592105263157915,
6.80807251039055));
#25335=CARTESIAN_POINT('Ctrl Pts',(-8.05403625519526,0.789473684210562,
4.65));
#25336=CARTESIAN_POINT('Ctrl Pts',(-9.29999999999998,0.986842105263191,
2.49192748960944));
#25337=CARTESIAN_POINT('Ctrl Pts',(-9.29999999999998,1.18421052631579,5.69460761603617E-16));
#25338=CARTESIAN_POINT('Ctrl Pts',(-9.29999999999998,1.38157894736841,-2.49192748960943));
#25339=CARTESIAN_POINT('Ctrl Pts',(-8.05403625519526,1.57894736842101,-4.64999999999998));
#25340=CARTESIAN_POINT('Ctrl Pts',(-6.80807251039055,1.77631578947369,-6.80807251039055));
#25341=CARTESIAN_POINT('Ctrl Pts',(-4.64999999999999,1.97368421052635,-8.05403625519526));
#25342=CARTESIAN_POINT('Ctrl Pts',(-2.49192748960944,2.17105263157896,-9.29999999999998));
#25343=CARTESIAN_POINT('Ctrl Pts',(-1.13892152320706E-15,2.36842105263158,
-9.29999999999998));
#25344=CARTESIAN_POINT('Ctrl Pts',(2.49192748960943,2.56578947368424,-9.29999999999998));
#25345=CARTESIAN_POINT('Ctrl Pts',(4.64999999999999,2.76315789473686,-8.05403625519526));
#25346=CARTESIAN_POINT('Ctrl Pts',(6.80807251039055,2.96052631578946,-6.80807251039056));
#25347=CARTESIAN_POINT('Ctrl Pts',(8.05403625519526,3.15789473684208,-4.64999999999999));
#25348=CARTESIAN_POINT('Ctrl Pts',(9.29999999999998,3.35526315789473,-2.49192748960944));
#25349=CARTESIAN_POINT('Ctrl Pts',(9.29999999999998,3.55263157894736,-1.70838228481046E-15));
#25350=CARTESIAN_POINT('Ctrl Pts',(9.29999999999998,3.75000000000001,2.49192748960943));
#25351=CARTESIAN_POINT('Ctrl Pts',(8.05403625519526,3.94736842105264,4.64999999999998));
#25352=CARTESIAN_POINT('Ctrl Pts',(6.80807251039055,4.14473684210529,6.80807251039055));
#25353=CARTESIAN_POINT('Ctrl Pts',(4.64999999999999,4.34210526315781,8.05403625519526));
#25354=CARTESIAN_POINT('Ctrl Pts',(2.49192748960944,4.53947368421051,9.29999999999998));
#25355=CARTESIAN_POINT('Ctrl Pts',(1.03229845019156E-28,4.73684210526315,
9.29999999999998));
#25356=CARTESIAN_POINT('Ctrl Pts',(-2.49192748960943,4.93421052631578,9.29999999999997));
#25357=CARTESIAN_POINT('Ctrl Pts',(-4.64999999999999,5.13157894736838,8.05403625519527));
#25358=CARTESIAN_POINT('Ctrl Pts',(-6.80807251039055,5.32894736842106,6.80807251039054));
#25359=CARTESIAN_POINT('Ctrl Pts',(-8.05403625519526,5.52631578947371,4.65));
#25360=CARTESIAN_POINT('Ctrl Pts',(-9.29999999999998,5.72368421052634,2.49192748960944));
#25361=CARTESIAN_POINT('Ctrl Pts',(-9.29999999999998,5.92105263157894,5.69460761603617E-16));
#25362=CARTESIAN_POINT('Ctrl Pts',(-9.29999999999998,6.11842105263156,-2.49192748960943));
#25363=CARTESIAN_POINT('Ctrl Pts',(-8.05403625519526,6.31578947368422,-4.64999999999998));
#25364=CARTESIAN_POINT('Ctrl Pts',(-6.80807251039055,6.51315789473683,-6.80807251039055));
#25365=CARTESIAN_POINT('Ctrl Pts',(-4.64999999999999,6.7105263157895,-8.05403625519525));
#25366=CARTESIAN_POINT('Ctrl Pts',(-2.49192748960944,6.90789473684211,-9.29999999999998));
#25367=CARTESIAN_POINT('Ctrl Pts',(-1.138921523207E-15,7.10526315789478,
-9.29999999999997));
#25368=CARTESIAN_POINT('Ctrl Pts',(2.49192748960943,7.30263157894738,-9.29999999999998));
#25369=CARTESIAN_POINT('Ctrl Pts',(4.64999999999999,7.50000000000006,-8.05403625519526));
#25370=CARTESIAN_POINT('Ctrl Pts',(6.80807251039055,7.69736842105261,-6.80807251039056));
#25371=CARTESIAN_POINT('Ctrl Pts',(8.05403625519526,7.89473684210523,-4.64999999999999));
#25372=CARTESIAN_POINT('Ctrl Pts',(9.29999999999998,8.09210526315788,-2.49192748960944));
#25373=CARTESIAN_POINT('Ctrl Pts',(9.29999999999998,8.28947368421051,-1.70838228481065E-15));
#25374=CARTESIAN_POINT('Ctrl Pts',(9.29999999999998,8.48684210526316,2.49192748960943));
#25375=CARTESIAN_POINT('Ctrl Pts',(8.05403625519526,8.68421052631579,4.64999999999998));
#25376=CARTESIAN_POINT('Ctrl Pts',(6.80807251039055,8.88157894736843,6.80807251039054));
#25377=CARTESIAN_POINT('Ctrl Pts',(4.64999999999999,9.07894736842096,8.05403625519526));
#25378=CARTESIAN_POINT('Ctrl Pts',(2.49192748960944,9.27631578947365,9.29999999999998));
#25379=CARTESIAN_POINT('Ctrl Pts',(1.57155883461998E-28,9.4736842105263,
9.29999999999998));
#25380=CARTESIAN_POINT('Ctrl Pts',(-2.49192748960943,9.67105263157893,9.29999999999998));
#25381=CARTESIAN_POINT('Ctrl Pts',(-4.64999999999999,9.86842105263153,8.05403625519526));
#25382=CARTESIAN_POINT('Ctrl Pts',(-6.80807251039055,10.0657894736842,6.80807251039055));
#25383=CARTESIAN_POINT('Ctrl Pts',(-8.05403625519526,10.2631578947369,4.65));
#25384=CARTESIAN_POINT('Ctrl Pts',(-9.29999999999998,10.4605263157895,2.49192748960944));
#25385=CARTESIAN_POINT('Ctrl Pts',(-9.29999999999998,10.6578947368421,5.6946076160342E-16));
#25386=CARTESIAN_POINT('Ctrl Pts',(-9.29999999999998,10.8552631578947,-2.49192748960943));
#25387=CARTESIAN_POINT('Ctrl Pts',(-8.05403625519526,11.0526315789474,-4.64999999999998));
#25388=CARTESIAN_POINT('Ctrl Pts',(-6.80807251039055,11.25,-6.80807251039055));
#25389=CARTESIAN_POINT('Ctrl Pts',(-4.64999999999999,11.4473684210527,-8.05403625519526));
#25390=CARTESIAN_POINT('Ctrl Pts',(-2.49192748960944,11.6447368421053,-9.29999999999999));
#25391=CARTESIAN_POINT('Ctrl Pts',(-1.13892152320696E-15,11.8421052631579,
-9.29999999999998));
#25392=CARTESIAN_POINT('Ctrl Pts',(2.49192748960943,12.0394736842105,-9.29999999999998));
#25393=CARTESIAN_POINT('Ctrl Pts',(4.64999999999999,12.2368421052632,-8.05403625519526));
#25394=CARTESIAN_POINT('Ctrl Pts',(6.80807251039055,12.4342105263158,-6.80807251039055));
#25395=CARTESIAN_POINT('Ctrl Pts',(8.05403625519526,12.6315789473684,-4.64999999999999));
#25396=CARTESIAN_POINT('Ctrl Pts',(9.29999999999998,12.828947368421,-2.49192748960944));
#25397=CARTESIAN_POINT('Ctrl Pts',(9.29999999999998,13.0263157894737,-1.70838228481065E-15));
#25398=CARTESIAN_POINT('Ctrl Pts',(9.29999999999998,13.2236842105263,2.49192748960943));
#25399=CARTESIAN_POINT('Ctrl Pts',(8.05403625519526,13.4210526315789,4.64999999999998));
#25400=CARTESIAN_POINT('Ctrl Pts',(6.80807251039055,13.6184210526316,6.80807251039054));
#25401=CARTESIAN_POINT('Ctrl Pts',(4.64999999999999,13.8157894736841,8.05403625519526));
#25402=CARTESIAN_POINT('Ctrl Pts',(2.49192748960944,14.0131578947368,9.29999999999998));
#25403=CARTESIAN_POINT('Ctrl Pts',(2.04918946082802E-28,14.2105263157895,
9.29999999999998));
#25404=CARTESIAN_POINT('Ctrl Pts',(-2.49192748960943,14.4078947368421,9.29999999999998));
#25405=CARTESIAN_POINT('Ctrl Pts',(-4.64999999999999,14.6052631578947,8.05403625519527));
#25406=CARTESIAN_POINT('Ctrl Pts',(-6.80807251039055,14.8026315789474,6.80807251039055));
#25407=CARTESIAN_POINT('Ctrl Pts',(-8.05403625519526,15.,4.65));
#25408=CARTESIAN_POINT('Ctrl Pts',(-9.29999999999998,15.1973684210526,2.49192748960944));
#25409=CARTESIAN_POINT('Ctrl Pts',(-9.29999999999998,15.3947368421052,5.69460761604603E-16));
#25410=CARTESIAN_POINT('Ctrl Pts',(-9.29999999999998,15.5921052631579,-2.49192748960943));
#25411=CARTESIAN_POINT('Ctrl Pts',(-8.05403625519526,15.7894736842105,-4.64999999999998));
#25412=CARTESIAN_POINT('Ctrl Pts',(-6.80807251039055,15.9868421052631,-6.80807251039055));
#25413=CARTESIAN_POINT('Ctrl Pts',(-4.64999999999999,16.1842105263158,-8.05403625519526));
#25414=CARTESIAN_POINT('Ctrl Pts',(-2.49192748960944,16.3815789473685,-9.29999999999998));
#25415=CARTESIAN_POINT('Ctrl Pts',(-1.13892152320691E-15,16.5789473684211,
-9.29999999999997));
#25416=CARTESIAN_POINT('Ctrl Pts',(2.49192748960943,16.7763157894737,-9.29999999999999));
#25417=CARTESIAN_POINT('Ctrl Pts',(4.64999999999999,16.9736842105264,-8.05403625519526));
#25418=CARTESIAN_POINT('Ctrl Pts',(6.80807251039055,17.1710526315789,-6.80807251039056));
#25419=CARTESIAN_POINT('Ctrl Pts',(8.05403625519526,17.3684210526315,-4.64999999999999));
#25420=CARTESIAN_POINT('Ctrl Pts',(9.29999999999998,17.5657894736842,-2.49192748960944));
#25421=CARTESIAN_POINT('Ctrl Pts',(9.29999999999998,17.7631578947368,-1.70838228481065E-15));
#25422=CARTESIAN_POINT('Ctrl Pts',(9.29999999999998,17.9605263157895,2.49192748960943));
#25423=CARTESIAN_POINT('Ctrl Pts',(8.05403625519526,18.1578947368421,4.64999999999999));
#25424=CARTESIAN_POINT('Ctrl Pts',(6.80807251039055,18.3552631578948,6.80807251039055));
#25425=CARTESIAN_POINT('Ctrl Pts',(4.64999999999999,18.5526315789473,8.05403625519527));
#25426=CARTESIAN_POINT('Ctrl Pts',(2.49192748960944,18.75,9.29999999999998));
#25427=CARTESIAN_POINT('Ctrl Pts',(2.58844984525644E-28,18.9473684210526,
9.29999999999998));
#25428=CARTESIAN_POINT('Ctrl Pts',(-2.49192748960943,19.1447368421052,9.29999999999998));
#25429=CARTESIAN_POINT('Ctrl Pts',(-4.64999999999999,19.3421052631578,8.05403625519526));
#25430=CARTESIAN_POINT('Ctrl Pts',(-6.80807251039055,19.5394736842105,6.80807251039055));
#25431=CARTESIAN_POINT('Ctrl Pts',(-8.05403625519526,19.7368421052632,4.65));
#25432=CARTESIAN_POINT('Ctrl Pts',(-9.29999999999998,19.9342105263158,2.49192748960944));
#25433=CARTESIAN_POINT('Ctrl Pts',(-9.29999999999998,20.1315789473684,5.694607616048E-16));
#25434=CARTESIAN_POINT('Ctrl Pts',(-9.29999999999998,20.328947368421,-2.49192748960943));
#25435=CARTESIAN_POINT('Ctrl Pts',(-8.05403625519526,20.5263157894737,-4.64999999999998));
#25436=CARTESIAN_POINT('Ctrl Pts',(-6.80807251039055,20.7236842105263,-6.80807251039055));
#25437=CARTESIAN_POINT('Ctrl Pts',(-4.64999999999999,20.921052631579,-8.05403625519526));
#25438=CARTESIAN_POINT('Ctrl Pts',(-2.49192748960944,21.1184210526316,-9.29999999999998));
#25439=CARTESIAN_POINT('Ctrl Pts',(-1.13892152320685E-15,21.3157894736842,
-9.29999999999998));
#25440=CARTESIAN_POINT('Ctrl Pts',(2.49192748960943,21.5131578947369,-9.29999999999998));
#25441=CARTESIAN_POINT('Ctrl Pts',(4.64999999999999,21.7105263157895,-8.05403625519526));
#25442=CARTESIAN_POINT('Ctrl Pts',(6.80807251039055,21.9078947368421,-6.80807251039055));
#25443=CARTESIAN_POINT('Ctrl Pts',(8.05403625519526,22.1052631578947,-4.64999999999999));
#25444=CARTESIAN_POINT('Ctrl Pts',(9.29999999999998,22.3026315789474,-2.49192748960944));
#25445=CARTESIAN_POINT('Ctrl Pts',(9.29999999999998,22.5,-1.70838228481046E-15));
#25446=CARTESIAN_POINT('Ctrl Pts',(9.29999999999998,22.6973684210527,2.49192748960943));
#25447=CARTESIAN_POINT('Ctrl Pts',(8.05403625519526,22.8947368421053,4.64999999999999));
#25448=CARTESIAN_POINT('Ctrl Pts',(6.80807251039055,23.0921052631579,6.80807251039054));
#25449=CARTESIAN_POINT('Ctrl Pts',(4.64999999999999,23.2894736842104,8.05403625519526));
#25450=CARTESIAN_POINT('Ctrl Pts',(2.49192748960944,23.4868421052631,9.29999999999996));
#25451=CARTESIAN_POINT('Ctrl Pts',(3.14311766923997E-28,23.6842105263158,
9.29999999999998));
#25452=CARTESIAN_POINT('Ctrl Pts',(-2.49192748960943,23.8815789473684,9.29999999999998));
#25453=CARTESIAN_POINT('Ctrl Pts',(-4.64999999999999,24.078947368421,8.05403625519527));
#25454=CARTESIAN_POINT('Ctrl Pts',(-6.80807251039055,24.2763157894737,6.80807251039055));
#25455=CARTESIAN_POINT('Ctrl Pts',(-8.05403625519526,24.4736842105263,4.65));
#25456=CARTESIAN_POINT('Ctrl Pts',(-9.29999999999998,24.671052631579,2.49192748960944));
#25457=CARTESIAN_POINT('Ctrl Pts',(-9.29999999999998,24.8684210526316,5.69460761603617E-16));
#25458=CARTESIAN_POINT('Ctrl Pts',(-9.29999999999998,25.0657894736842,-2.49192748960943));
#25459=CARTESIAN_POINT('Ctrl Pts',(-8.05403625519526,25.2631578947368,-4.64999999999999));
#25460=CARTESIAN_POINT('Ctrl Pts',(-6.80807251039055,25.4605263157894,-6.80807251039055));
#25461=CARTESIAN_POINT('Ctrl Pts',(-4.64999999999999,25.6578947368421,-8.05403625519526));
#25462=CARTESIAN_POINT('Ctrl Pts',(-2.49192748960944,25.8552631578947,-9.29999999999998));
#25463=CARTESIAN_POINT('Ctrl Pts',(-1.1389215232068E-15,26.0526315789474,
-9.29999999999997));
#25464=CARTESIAN_POINT('Ctrl Pts',(2.49192748960943,26.25,-9.29999999999998));
#25465=CARTESIAN_POINT('Ctrl Pts',(4.64999999999999,26.4473684210527,-8.05403625519526));
#25466=CARTESIAN_POINT('Ctrl Pts',(6.80807251039055,26.6447368421052,-6.80807251039056));
#25467=CARTESIAN_POINT('Ctrl Pts',(8.05403625519526,26.8421052631579,-4.64999999999999));
#25468=CARTESIAN_POINT('Ctrl Pts',(9.29999999999998,27.0394736842105,-2.49192748960945));
#25469=CARTESIAN_POINT('Ctrl Pts',(9.29999999999998,27.2368421052632,-1.70838228481046E-15));
#25470=CARTESIAN_POINT('Ctrl Pts',(9.29999999999998,27.4342105263158,2.49192748960943));
#25471=CARTESIAN_POINT('Ctrl Pts',(8.05403625519526,27.6315789473685,4.64999999999999));
#25472=CARTESIAN_POINT('Ctrl Pts',(6.80807251039055,27.8289473684211,6.80807251039055));
#25473=CARTESIAN_POINT('Ctrl Pts',(4.64999999999999,28.0263157894737,8.05403625519527));
#25474=CARTESIAN_POINT('Ctrl Pts',(2.49192748960944,28.2236842105263,9.29999999999998));
#25475=CARTESIAN_POINT('Ctrl Pts',(3.60534085589291E-28,28.4210526315789,
9.29999999999998));
#25476=CARTESIAN_POINT('Ctrl Pts',(-2.49192748960943,28.6184210526316,9.29999999999997));
#25477=CARTESIAN_POINT('Ctrl Pts',(-4.64999999999999,28.8157894736841,8.05403625519526));
#25478=CARTESIAN_POINT('Ctrl Pts',(-6.80807251039055,29.0131578947368,6.80807251039054));
#25479=CARTESIAN_POINT('Ctrl Pts',(-8.05403625519526,29.2105263157895,4.65));
#25480=CARTESIAN_POINT('Ctrl Pts',(-9.29999999999998,29.4078947368421,2.49192748960944));
#25481=CARTESIAN_POINT('Ctrl Pts',(-9.29999999999998,29.6052631578947,5.69460761603617E-16));
#25482=CARTESIAN_POINT('Ctrl Pts',(-9.29999999999998,29.8026315789473,-2.49192748960943));
#25483=CARTESIAN_POINT('Ctrl Pts',(-8.05403625519526,30.,-4.64999999999999));
#25484=CARTESIAN_POINT('Ctrl Pts',(-6.80807251039055,30.1973684210526,-6.80807251039055));
#25485=CARTESIAN_POINT('Ctrl Pts',(-4.64999999999999,30.3947368421054,-8.05403625519526));
#25486=CARTESIAN_POINT('Ctrl Pts',(-2.49192748960944,30.5921052631579,-9.29999999999998));
#25487=CARTESIAN_POINT('Ctrl Pts',(-1.13892152320674E-15,30.7894736842105,
-9.29999999999998));
#25488=CARTESIAN_POINT('Ctrl Pts',(2.49192748960943,30.9868421052632,-9.29999999999998));
#25489=CARTESIAN_POINT('Ctrl Pts',(4.64999999999999,31.1842105263158,-8.05403625519526));
#25490=CARTESIAN_POINT('Ctrl Pts',(6.80807251039055,31.3815789473684,-6.80807251039055));
#25491=CARTESIAN_POINT('Ctrl Pts',(8.05403625519526,31.578947368421,-4.64999999999999));
#25492=CARTESIAN_POINT('Ctrl Pts',(9.29999999999998,31.7763157894737,-2.49192748960944));
#25493=CARTESIAN_POINT('Ctrl Pts',(9.29999999999998,31.9736842105263,-1.70838228481046E-15));
#25494=CARTESIAN_POINT('Ctrl Pts',(9.29999999999998,32.1710526315789,2.49192748960943));
#25495=CARTESIAN_POINT('Ctrl Pts',(8.05403625519526,32.3684210526316,4.64999999999999));
#25496=CARTESIAN_POINT('Ctrl Pts',(6.80807251039055,32.5657894736842,6.80807251039054));
#25497=CARTESIAN_POINT('Ctrl Pts',(4.64999999999999,32.7631578947368,8.05403625519526));
#25498=CARTESIAN_POINT('Ctrl Pts',(2.49192748960944,32.9605263157894,9.29999999999998));
#25499=CARTESIAN_POINT('Ctrl Pts',(4.14460124032133E-28,33.1578947368421,
9.29999999999998));
#25500=CARTESIAN_POINT('Ctrl Pts',(-2.49192748960943,33.3552631578947,9.29999999999998));
#25501=CARTESIAN_POINT('Ctrl Pts',(-4.64999999999999,33.5526315789473,8.05403625519527));
#25502=CARTESIAN_POINT('Ctrl Pts',(-6.80807251039055,33.75,6.80807251039055));
#25503=CARTESIAN_POINT('Ctrl Pts',(-8.05403625519526,33.9473684210527,4.64999999999999));
#25504=CARTESIAN_POINT('Ctrl Pts',(-9.29999999999998,34.1447368421052,2.49192748960944));
#25505=CARTESIAN_POINT('Ctrl Pts',(-9.29999999999998,34.3421052631579,5.69460761604603E-16));
#25506=CARTESIAN_POINT('Ctrl Pts',(-9.29999999999998,34.5394736842105,-2.49192748960943));
#25507=CARTESIAN_POINT('Ctrl Pts',(-8.05403625519526,34.7368421052631,-4.64999999999999));
#25508=CARTESIAN_POINT('Ctrl Pts',(-6.80807251039055,34.9342105263158,-6.80807251039055));
#25509=CARTESIAN_POINT('Ctrl Pts',(-4.64999999999999,35.1315789473685,-8.05403625519526));
#25510=CARTESIAN_POINT('Ctrl Pts',(-2.49192748960944,35.3289473684211,-9.29999999999999));
#25511=CARTESIAN_POINT('Ctrl Pts',(-1.1389215232067E-15,35.5263157894737,
-9.29999999999998));
#25512=CARTESIAN_POINT('Ctrl Pts',(2.49192748960943,35.7236842105263,-9.29999999999998));
#25513=CARTESIAN_POINT('Ctrl Pts',(4.64999999999999,35.921052631579,-8.05403625519525));
#25514=CARTESIAN_POINT('Ctrl Pts',(6.80807251039055,36.1184210526315,-6.80807251039056));
#25515=CARTESIAN_POINT('Ctrl Pts',(8.05403625519526,36.3157894736842,-4.64999999999999));
#25516=CARTESIAN_POINT('Ctrl Pts',(9.29999999999998,36.5131578947368,-2.49192748960944));
#25517=CARTESIAN_POINT('Ctrl Pts',(9.29999999999998,36.7105263157895,-1.70838228481065E-15));
#25518=CARTESIAN_POINT('Ctrl Pts',(9.29999999999998,36.9078947368421,2.49192748960943));
#25519=CARTESIAN_POINT('Ctrl Pts',(8.05403625519526,37.1052631578948,4.64999999999999));
#25520=CARTESIAN_POINT('Ctrl Pts',(6.80807251039055,37.3026315789473,6.80807251039055));
#25521=CARTESIAN_POINT('Ctrl Pts',(4.64999999999999,37.5,8.05403625519526));
#25522=CARTESIAN_POINT('Ctrl Pts',(2.49192748960944,37.6973684210526,9.29999999999998));
#25523=CARTESIAN_POINT('Ctrl Pts',(4.65304674563956E-28,37.8947368421053,
9.29999999999998));
#25524=CARTESIAN_POINT('Ctrl Pts',(-2.49192748960943,38.0921052631579,9.29999999999998));
#25525=CARTESIAN_POINT('Ctrl Pts',(-4.64999999999999,38.2894736842104,8.05403625519526));
#25526=CARTESIAN_POINT('Ctrl Pts',(-6.80807251039055,38.4868421052632,6.80807251039054));
#25527=CARTESIAN_POINT('Ctrl Pts',(-8.05403625519526,38.6842105263158,4.64999999999999));
#25528=CARTESIAN_POINT('Ctrl Pts',(-9.29999999999998,38.8815789473684,2.49192748960944));
#25529=CARTESIAN_POINT('Ctrl Pts',(-9.29999999999998,39.078947368421,5.69460761604603E-16));
#25530=CARTESIAN_POINT('Ctrl Pts',(-9.29999999999998,39.2763157894737,-2.49192748960943));
#25531=CARTESIAN_POINT('Ctrl Pts',(-8.05403625519526,39.4736842105263,-4.64999999999999));
#25532=CARTESIAN_POINT('Ctrl Pts',(-6.80807251039055,39.6710526315789,-6.80807251039055));
#25533=CARTESIAN_POINT('Ctrl Pts',(-4.64999999999999,39.8684210526317,-8.05403625519526));
#25534=CARTESIAN_POINT('Ctrl Pts',(-2.49192748960944,40.0657894736842,-9.29999999999998));
#25535=CARTESIAN_POINT('Ctrl Pts',(-1.13892152320665E-15,40.2631578947368,
-9.29999999999998));
#25536=CARTESIAN_POINT('Ctrl Pts',(2.49192748960943,40.4605263157895,-9.29999999999999));
#25537=CARTESIAN_POINT('Ctrl Pts',(4.64999999999999,40.6578947368421,-8.05403625519526));
#25538=CARTESIAN_POINT('Ctrl Pts',(6.80807251039055,40.8552631578947,-6.80807251039056));
#25539=CARTESIAN_POINT('Ctrl Pts',(8.05403625519526,41.0526315789473,-4.64999999999999));
#25540=CARTESIAN_POINT('Ctrl Pts',(9.29999999999998,41.25,-2.49192748960944));
#25541=CARTESIAN_POINT('Ctrl Pts',(9.29999999999998,41.4473684210526,-1.70838228481085E-15));
#25542=CARTESIAN_POINT('Ctrl Pts',(9.29999999999998,41.6447368421053,2.49192748960943));
#25543=CARTESIAN_POINT('Ctrl Pts',(8.05403625519526,41.8421052631579,4.64999999999998));
#25544=CARTESIAN_POINT('Ctrl Pts',(6.80807251039055,42.0394736842106,6.80807251039054));
#25545=CARTESIAN_POINT('Ctrl Pts',(4.64999999999999,42.2368421052631,8.05403625519526));
#25546=CARTESIAN_POINT('Ctrl Pts',(2.49192748960944,42.4342105263158,9.29999999999996));
#25547=CARTESIAN_POINT('Ctrl Pts',(5.17689969051289E-28,42.6315789473684,
9.29999999999998));
#25548=CARTESIAN_POINT('Ctrl Pts',(-2.49192748960943,42.828947368421,9.29999999999998));
#25549=CARTESIAN_POINT('Ctrl Pts',(-4.64999999999999,43.0263157894736,8.05403625519526));
#25550=CARTESIAN_POINT('Ctrl Pts',(-6.80807251039055,43.2236842105263,6.80807251039055));
#25551=CARTESIAN_POINT('Ctrl Pts',(-8.05403625519526,43.421052631579,4.64999999999999));
#25552=CARTESIAN_POINT('Ctrl Pts',(-9.29999999999998,43.6184210526316,2.49192748960944));
#25553=CARTESIAN_POINT('Ctrl Pts',(-9.29999999999998,43.8157894736842,5.69460761603617E-16));
#25554=CARTESIAN_POINT('Ctrl Pts',(-9.29999999999998,44.0131578947368,-2.49192748960943));
#25555=CARTESIAN_POINT('Ctrl Pts',(-8.05403625519526,44.2105263157894,-4.64999999999999));
#25556=CARTESIAN_POINT('Ctrl Pts',(-6.80807251039055,44.4078947368421,-6.80807251039055));
#25557=CARTESIAN_POINT('Ctrl Pts',(-4.64999999999999,44.6052631578948,-8.05403625519526));
#25558=CARTESIAN_POINT('Ctrl Pts',(-2.49192748960944,44.8026315789474,-9.29999999999998));
#25559=CARTESIAN_POINT('Ctrl Pts',(-1.1389215232066E-15,45.,-9.29999999999998));
#25560=CARTESIAN_POINT('Ctrl Pts',(2.49192748960943,45.1973684210527,-9.29999999999998));
#25561=CARTESIAN_POINT('Ctrl Pts',(4.64999999999999,45.3947368421053,-8.05403625519525));
#25562=CARTESIAN_POINT('Ctrl Pts',(6.80807251039055,45.5921052631579,-6.80807251039055));
#25563=CARTESIAN_POINT('Ctrl Pts',(8.05403625519526,45.7894736842105,-4.64999999999999));
#25564=CARTESIAN_POINT('Ctrl Pts',(9.29999999999998,45.9868421052631,-2.49192748960944));
#25565=CARTESIAN_POINT('Ctrl Pts',(9.29999999999998,46.1842105263158,-1.70838228481046E-15));
#25566=CARTESIAN_POINT('Ctrl Pts',(9.29999999999998,46.3815789473684,2.49192748960943));
#25567=CARTESIAN_POINT('Ctrl Pts',(8.05403625519526,46.5789473684211,4.64999999999998));
#25568=CARTESIAN_POINT('Ctrl Pts',(6.80807251039055,46.7763157894737,6.80807251039054));
#25569=CARTESIAN_POINT('Ctrl Pts',(4.64999999999999,46.9736842105263,8.05403625519526));
#25570=CARTESIAN_POINT('Ctrl Pts',(2.49192748960944,47.1710526315789,9.29999999999996));
#25571=CARTESIAN_POINT('Ctrl Pts',(5.73156751449641E-28,47.3684210526316,
9.29999999999999));
#25572=CARTESIAN_POINT('Ctrl Pts',(-2.49192748960943,47.5657894736841,9.29999999999998));
#25573=CARTESIAN_POINT('Ctrl Pts',(-4.64999999999999,47.7631578947367,8.05403625519526));
#25574=CARTESIAN_POINT('Ctrl Pts',(-6.80807251039055,47.9605263157895,6.80807251039055));
#25575=CARTESIAN_POINT('Ctrl Pts',(-8.05403625519526,48.1578947368421,4.64999999999999));
#25576=CARTESIAN_POINT('Ctrl Pts',(-9.29999999999998,48.3552631578947,2.49192748960944));
#25577=CARTESIAN_POINT('Ctrl Pts',(-9.29999999999998,48.5526315789474,5.6946076160342E-16));
#25578=CARTESIAN_POINT('Ctrl Pts',(-9.29999999999998,48.75,-2.49192748960943));
#25579=CARTESIAN_POINT('Ctrl Pts',(-8.05403625519526,48.9473684210526,-4.64999999999999));
#25580=CARTESIAN_POINT('Ctrl Pts',(-6.80807251039055,49.1447368421053,-6.80807251039055));
#25581=CARTESIAN_POINT('Ctrl Pts',(-4.64999999999999,49.342105263158,-8.05403625519525));
#25582=CARTESIAN_POINT('Ctrl Pts',(-2.49192748960944,49.5394736842105,-9.29999999999998));
#25583=CARTESIAN_POINT('Ctrl Pts',(-1.13892152320654E-15,49.7368421052632,
-9.29999999999998));
#25584=CARTESIAN_POINT('Ctrl Pts',(2.49192748960943,49.9342105263158,-9.29999999999998));
#25585=CARTESIAN_POINT('Ctrl Pts',(4.64999999999999,50.1315789473684,-8.05403625519526));
#25586=CARTESIAN_POINT('Ctrl Pts',(6.80807251039055,50.328947368421,-6.80807251039056));
#25587=CARTESIAN_POINT('Ctrl Pts',(8.05403625519526,50.5263157894736,-4.64999999999999));
#25588=CARTESIAN_POINT('Ctrl Pts',(9.29999999999998,50.7236842105263,-2.49192748960944));
#25589=CARTESIAN_POINT('Ctrl Pts',(9.29999999999998,50.9210526315789,-1.70838228480937E-15));
#25590=CARTESIAN_POINT('Ctrl Pts',(9.29999999999998,51.1184210526316,2.49192748960943));
#25591=CARTESIAN_POINT('Ctrl Pts',(8.05403625519526,51.3157894736842,4.64999999999998));
#25592=CARTESIAN_POINT('Ctrl Pts',(6.80807251039055,51.5131578947368,6.80807251039055));
#25593=CARTESIAN_POINT('Ctrl Pts',(4.64999999999999,51.7105263157894,8.05403625519526));
#25594=CARTESIAN_POINT('Ctrl Pts',(2.49192748960944,51.9078947368421,9.29999999999998));
#25595=CARTESIAN_POINT('Ctrl Pts',(6.28623533847994E-28,52.1052631578947,
9.29999999999998));
#25596=CARTESIAN_POINT('Ctrl Pts',(-2.49192748960943,52.3026315789474,9.29999999999997));
#25597=CARTESIAN_POINT('Ctrl Pts',(-4.64999999999999,52.5,8.05403625519526));
#25598=CARTESIAN_POINT('Ctrl Pts',(-6.80807251039055,52.6973684210526,6.80807251039054));
#25599=CARTESIAN_POINT('Ctrl Pts',(-8.05403625519526,52.8947368421053,4.64999999999999));
#25600=CARTESIAN_POINT('Ctrl Pts',(-9.29999999999998,53.0921052631579,2.49192748960944));
#25601=CARTESIAN_POINT('Ctrl Pts',(-9.29999999999998,53.2894736842105,5.69460761604603E-16));
#25602=CARTESIAN_POINT('Ctrl Pts',(-9.29999999999998,53.4868421052631,-2.49192748960943));
#25603=CARTESIAN_POINT('Ctrl Pts',(-8.05403625519526,53.6842105263158,-4.64999999999998));
#25604=CARTESIAN_POINT('Ctrl Pts',(-6.80807251039055,53.8815789473684,-6.80807251039055));
#25605=CARTESIAN_POINT('Ctrl Pts',(-4.64999999999999,54.0789473684211,-8.05403625519526));
#25606=CARTESIAN_POINT('Ctrl Pts',(-2.49192748960944,54.2763157894737,-9.29999999999999));
#25607=CARTESIAN_POINT('Ctrl Pts',(-1.13892152320649E-15,54.4736842105263,
-9.29999999999998));
#25608=CARTESIAN_POINT('Ctrl Pts',(2.49192748960943,54.671052631579,-9.29999999999998));
#25609=CARTESIAN_POINT('Ctrl Pts',(4.64999999999999,54.8684210526317,-8.05403625519525));
#25610=CARTESIAN_POINT('Ctrl Pts',(6.80807251039055,55.0657894736842,-6.80807251039055));
#25611=CARTESIAN_POINT('Ctrl Pts',(8.05403625519526,55.2631578947368,-4.64999999999999));
#25612=CARTESIAN_POINT('Ctrl Pts',(9.29999999999998,55.4605263157895,-2.49192748960945));
#25613=CARTESIAN_POINT('Ctrl Pts',(9.29999999999998,55.6578947368421,-1.70838228480947E-15));
#25614=CARTESIAN_POINT('Ctrl Pts',(9.29999999999998,55.8552631578947,2.49192748960943));
#25615=CARTESIAN_POINT('Ctrl Pts',(8.05403625519526,56.0526315789474,4.64999999999998));
#25616=CARTESIAN_POINT('Ctrl Pts',(6.80807251039055,56.25,6.80807251039054));
#25617=CARTESIAN_POINT('Ctrl Pts',(4.64999999999999,56.4473684210526,8.05403625519526));
#25618=CARTESIAN_POINT('Ctrl Pts',(2.49192748960944,56.6447368421052,9.29999999999998));
#25619=CARTESIAN_POINT('Ctrl Pts',(6.74845852513287E-28,56.8421052631579,
9.29999999999999));
#25620=CARTESIAN_POINT('Ctrl Pts',(-2.49192748960943,57.0394736842105,9.29999999999998));
#25621=CARTESIAN_POINT('Ctrl Pts',(-4.64999999999999,57.2368421052632,8.05403625519526));
#25622=CARTESIAN_POINT('Ctrl Pts',(-6.80807251039055,57.4342105263158,6.80807251039055));
#25623=CARTESIAN_POINT('Ctrl Pts',(-8.05403625519526,57.6315789473684,4.64999999999999));
#25624=CARTESIAN_POINT('Ctrl Pts',(-9.29999999999998,57.8289473684211,2.49192748960944));
#25625=CARTESIAN_POINT('Ctrl Pts',(-9.29999999999998,58.0263157894737,5.69460761604603E-16));
#25626=CARTESIAN_POINT('Ctrl Pts',(-9.29999999999998,58.2236842105263,-2.49192748960943));
#25627=CARTESIAN_POINT('Ctrl Pts',(-8.05403625519526,58.4210526315789,-4.64999999999998));
#25628=CARTESIAN_POINT('Ctrl Pts',(-6.80807251039055,58.6184210526316,-6.80807251039055));
#25629=CARTESIAN_POINT('Ctrl Pts',(-4.64999999999999,58.8157894736843,-8.05403625519525));
#25630=CARTESIAN_POINT('Ctrl Pts',(-2.49192748960944,59.0131578947368,-9.29999999999999));
#25631=CARTESIAN_POINT('Ctrl Pts',(-1.13892152320644E-15,59.2105263157895,
-9.29999999999998));
#25632=CARTESIAN_POINT('Ctrl Pts',(2.49192748960943,59.4078947368421,-9.29999999999999));
#25633=CARTESIAN_POINT('Ctrl Pts',(4.64999999999999,59.6052631578948,-8.05403625519526));
#25634=CARTESIAN_POINT('Ctrl Pts',(6.80807251039055,59.8026315789474,-6.80807251039056));
#25635=CARTESIAN_POINT('Ctrl Pts',(8.05403625519526,60.,-4.64999999999999));
#25636=CARTESIAN_POINT('Ctrl Pts',(9.29999999999998,60.1973684210526,-2.49192748960944));
#25637=CARTESIAN_POINT('Ctrl Pts',(9.29999999999998,60.3947368421052,-1.70838228480947E-15));
#25638=CARTESIAN_POINT('Ctrl Pts',(9.29999999999998,60.5921052631579,2.49192748960943));
#25639=CARTESIAN_POINT('Ctrl Pts',(8.05403625519526,60.7894736842106,4.64999999999998));
#25640=CARTESIAN_POINT('Ctrl Pts',(6.80807251039055,60.9868421052632,6.80807251039055));
#25641=CARTESIAN_POINT('Ctrl Pts',(4.64999999999999,61.1842105263157,8.05403625519526));
#25642=CARTESIAN_POINT('Ctrl Pts',(2.49192748960944,61.3815789473684,9.29999999999998));
#25643=CARTESIAN_POINT('Ctrl Pts',(7.21068171178581E-28,61.578947368421,
9.29999999999998));
#25644=CARTESIAN_POINT('Ctrl Pts',(-2.49192748960943,61.7763157894737,9.29999999999998));
#25645=CARTESIAN_POINT('Ctrl Pts',(-4.64999999999999,61.9736842105263,8.05403625519526));
#25646=CARTESIAN_POINT('Ctrl Pts',(-6.80807251039055,62.171052631579,6.80807251039054));
#25647=CARTESIAN_POINT('Ctrl Pts',(-8.05403625519526,62.3684210526316,4.64999999999999));
#25648=CARTESIAN_POINT('Ctrl Pts',(-9.29999999999998,62.5657894736842,2.49192748960944));
#25649=CARTESIAN_POINT('Ctrl Pts',(-9.29999999999998,62.7631578947368,5.69460761604012E-16));
#25650=CARTESIAN_POINT('Ctrl Pts',(-9.29999999999998,62.9605263157895,-2.49192748960943));
#25651=CARTESIAN_POINT('Ctrl Pts',(-8.05403625519526,63.1578947368421,-4.64999999999998));
#25652=CARTESIAN_POINT('Ctrl Pts',(-6.80807251039055,63.3552631578947,-6.80807251039055));
#25653=CARTESIAN_POINT('Ctrl Pts',(-4.64999999999999,63.5526315789474,-8.05403625519526));
#25654=CARTESIAN_POINT('Ctrl Pts',(-2.49192748960944,63.75,-9.29999999999998));
#25655=CARTESIAN_POINT('Ctrl Pts',(-1.13892152320638E-15,63.9473684210526,
-9.29999999999998));
#25656=CARTESIAN_POINT('Ctrl Pts',(2.49192748960943,64.1447368421052,-9.29999999999999));
#25657=CARTESIAN_POINT('Ctrl Pts',(4.64999999999999,64.342105263158,-8.05403625519526));
#25658=CARTESIAN_POINT('Ctrl Pts',(6.80807251039055,64.5394736842105,-6.80807251039056));
#25659=CARTESIAN_POINT('Ctrl Pts',(8.05403625519526,64.7368421052632,-4.64999999999999));
#25660=CARTESIAN_POINT('Ctrl Pts',(9.29999999999998,64.9342105263157,-2.49192748960944));
#25661=CARTESIAN_POINT('Ctrl Pts',(9.29999999999998,65.1315789473684,-1.70838228480937E-15));
#25662=CARTESIAN_POINT('Ctrl Pts',(9.29999999999998,65.3289473684211,2.49192748960943));
#25663=CARTESIAN_POINT('Ctrl Pts',(8.05403625519526,65.5263157894736,4.64999999999998));
#25664=CARTESIAN_POINT('Ctrl Pts',(6.80807251039055,65.7236842105263,6.80807251039054));
#25665=CARTESIAN_POINT('Ctrl Pts',(4.64999999999999,65.9210526315789,8.05403625519526));
#25666=CARTESIAN_POINT('Ctrl Pts',(2.49192748960944,66.1184210526316,9.29999999999996));
#25667=CARTESIAN_POINT('Ctrl Pts',(7.71912721710404E-28,66.3157894736842,
9.29999999999999));
#25668=CARTESIAN_POINT('Ctrl Pts',(-2.49192748960943,66.5131578947368,9.29999999999998));
#25669=CARTESIAN_POINT('Ctrl Pts',(-4.64999999999999,66.7105263157895,8.05403625519526));
#25670=CARTESIAN_POINT('Ctrl Pts',(-6.80807251039055,66.9078947368421,6.80807251039055));
#25671=CARTESIAN_POINT('Ctrl Pts',(-8.05403625519526,67.1052631578947,4.65));
#25672=CARTESIAN_POINT('Ctrl Pts',(-9.29999999999998,67.3026315789474,2.49192748960944));
#25673=CARTESIAN_POINT('Ctrl Pts',(-9.29999999999998,67.5,5.69460761603617E-16));
#25674=CARTESIAN_POINT('Ctrl Pts',(-9.29999999999998,67.6973684210526,-2.49192748960943));
#25675=CARTESIAN_POINT('Ctrl Pts',(-8.05403625519526,67.8947368421053,-4.64999999999998));
#25676=CARTESIAN_POINT('Ctrl Pts',(-6.80807251039055,68.0921052631578,-6.80807251039055));
#25677=CARTESIAN_POINT('Ctrl Pts',(-4.64999999999999,68.2894736842105,-8.05403625519525));
#25678=CARTESIAN_POINT('Ctrl Pts',(-2.49192748960944,68.4868421052632,-9.29999999999998));
#25679=CARTESIAN_POINT('Ctrl Pts',(-1.13892152320634E-15,68.6842105263158,
-9.29999999999998));
#25680=CARTESIAN_POINT('Ctrl Pts',(2.49192748960943,68.8815789473684,-9.29999999999998));
#25681=CARTESIAN_POINT('Ctrl Pts',(4.64999999999999,69.078947368421,-8.05403625519526));
#25682=CARTESIAN_POINT('Ctrl Pts',(6.80807251039055,69.2763157894736,-6.80807251039055));
#25683=CARTESIAN_POINT('Ctrl Pts',(8.05403625519526,69.4736842105263,-4.64999999999999));
#25684=CARTESIAN_POINT('Ctrl Pts',(9.29999999999998,69.6710526315789,-2.49192748960944));
#25685=CARTESIAN_POINT('Ctrl Pts',(9.29999999999998,69.8684210526316,-1.70838228480927E-15));
#25686=CARTESIAN_POINT('Ctrl Pts',(9.29999999999998,70.0657894736842,2.49192748960943));
#25687=CARTESIAN_POINT('Ctrl Pts',(8.05403625519526,70.2631578947368,4.64999999999998));
#25688=CARTESIAN_POINT('Ctrl Pts',(6.80807251039055,70.4605263157895,6.80807251039055));
#25689=CARTESIAN_POINT('Ctrl Pts',(4.64999999999999,70.6578947368421,8.05403625519526));
#25690=CARTESIAN_POINT('Ctrl Pts',(2.49192748960944,70.8552631578948,9.29999999999998));
#25691=CARTESIAN_POINT('Ctrl Pts',(8.28920248064266E-28,71.0526315789473,
9.29999999999998));
#25692=CARTESIAN_POINT('Ctrl Pts',(-2.49192748960943,71.25,9.29999999999998));
#25693=CARTESIAN_POINT('Ctrl Pts',(-4.64999999999999,71.4473684210526,8.05403625519526));
#25694=CARTESIAN_POINT('Ctrl Pts',(-6.80807251039055,71.6447368421052,6.80807251039055));
#25695=CARTESIAN_POINT('Ctrl Pts',(-8.05403625519526,71.8421052631578,4.65));
#25696=CARTESIAN_POINT('Ctrl Pts',(-9.29999999999998,72.0394736842105,2.49192748960944));
#25697=CARTESIAN_POINT('Ctrl Pts',(-9.29999999999998,72.2368421052632,5.69460761604209E-16));
#25698=CARTESIAN_POINT('Ctrl Pts',(-9.29999999999998,72.4342105263157,-2.49192748960943));
#25699=CARTESIAN_POINT('Ctrl Pts',(-8.05403625519526,72.6315789473684,-4.64999999999998));
#25700=CARTESIAN_POINT('Ctrl Pts',(-6.80807251039055,72.828947368421,-6.80807251039055));
#25701=CARTESIAN_POINT('Ctrl Pts',(-4.64999999999999,73.0263157894737,-8.05403625519526));
#25702=CARTESIAN_POINT('Ctrl Pts',(-2.49192748960944,73.2236842105263,-9.29999999999998));
#25703=CARTESIAN_POINT('Ctrl Pts',(-1.13892152320628E-15,73.4210526315789,
-9.29999999999998));
#25704=CARTESIAN_POINT('Ctrl Pts',(2.49192748960943,73.6184210526315,-9.29999999999998));
#25705=CARTESIAN_POINT('Ctrl Pts',(4.64999999999999,73.8157894736842,-8.05403625519526));
#25706=CARTESIAN_POINT('Ctrl Pts',(6.80807251039055,74.0131578947368,-6.80807251039056));
#25707=CARTESIAN_POINT('Ctrl Pts',(8.05403625519526,74.2105263157895,-4.64999999999999));
#25708=CARTESIAN_POINT('Ctrl Pts',(9.29999999999998,74.4078947368421,-2.49192748960944));
#25709=CARTESIAN_POINT('Ctrl Pts',(9.29999999999998,74.6052631578947,-1.70838228480937E-15));
#25710=CARTESIAN_POINT('Ctrl Pts',(9.29999999999998,74.8026315789473,2.49192748960943));
#25711=CARTESIAN_POINT('Ctrl Pts',(8.05403625519526,75.,4.64999999999998));
#25712=CARTESIAN_POINT('Ctrl Pts',(6.80807251039055,75.1973684210526,6.80807251039055));
#25713=CARTESIAN_POINT('Ctrl Pts',(4.64999999999999,75.3947368421053,8.05403625519526));
#25714=CARTESIAN_POINT('Ctrl Pts',(2.49192748960944,75.5921052631579,9.29999999999998));
#25715=CARTESIAN_POINT('Ctrl Pts',(8.87468518373638E-28,75.7894736842105,
9.29999999999998));
#25716=CARTESIAN_POINT('Ctrl Pts',(-2.49192748960943,75.9868421052632,9.29999999999997));
#25717=CARTESIAN_POINT('Ctrl Pts',(-4.64999999999999,76.1842105263158,8.05403625519527));
#25718=CARTESIAN_POINT('Ctrl Pts',(-6.80807251039055,76.3815789473684,6.80807251039055));
#25719=CARTESIAN_POINT('Ctrl Pts',(-8.05403625519526,76.578947368421,4.65));
#25720=CARTESIAN_POINT('Ctrl Pts',(-9.29999999999998,76.7763157894737,2.49192748960944));
#25721=CARTESIAN_POINT('Ctrl Pts',(-9.29999999999998,76.9736842105263,5.69460761603519E-16));
#25722=CARTESIAN_POINT('Ctrl Pts',(-9.29999999999998,77.1710526315789,-2.49192748960943));
#25723=CARTESIAN_POINT('Ctrl Pts',(-8.05403625519526,77.3684210526316,-4.64999999999998));
#25724=CARTESIAN_POINT('Ctrl Pts',(-6.80807251039055,77.5657894736842,-6.80807251039055));
#25725=CARTESIAN_POINT('Ctrl Pts',(-4.64999999999999,77.7631578947368,-8.05403625519525));
#25726=CARTESIAN_POINT('Ctrl Pts',(-2.49192748960944,77.9605263157894,-9.29999999999999));
#25727=CARTESIAN_POINT('Ctrl Pts',(-1.13892152320623E-15,78.1578947368421,
-9.29999999999997));
#25728=CARTESIAN_POINT('Ctrl Pts',(2.49192748960943,78.3552631578947,-9.29999999999998));
#25729=CARTESIAN_POINT('Ctrl Pts',(4.64999999999999,78.5526315789473,-8.05403625519526));
#25730=CARTESIAN_POINT('Ctrl Pts',(6.80807251039055,78.75,-6.80807251039055));
#25731=CARTESIAN_POINT('Ctrl Pts',(8.05403625519526,78.9473684210526,-4.64999999999999));
#25732=CARTESIAN_POINT('Ctrl Pts',(9.29999999999998,79.1447368421052,-2.49192748960944));
#25733=CARTESIAN_POINT('Ctrl Pts',(9.29999999999998,79.3421052631579,-1.70838228480937E-15));
#25734=CARTESIAN_POINT('Ctrl Pts',(9.29999999999998,79.5394736842105,2.49192748960943));
#25735=CARTESIAN_POINT('Ctrl Pts',(8.05403625519526,79.7368421052631,4.64999999999998));
#25736=CARTESIAN_POINT('Ctrl Pts',(6.80807251039055,79.9342105263157,6.80807251039054));
#25737=CARTESIAN_POINT('Ctrl Pts',(4.64999999999999,80.1315789473684,8.05403625519526));
#25738=CARTESIAN_POINT('Ctrl Pts',(2.49192748960944,80.328947368421,9.29999999999998));
#25739=CARTESIAN_POINT('Ctrl Pts',(9.33690837038932E-28,80.5263157894737,
9.29999999999998));
#25740=CARTESIAN_POINT('Ctrl Pts',(-2.49192748960943,80.7236842105263,9.29999999999998));
#25741=CARTESIAN_POINT('Ctrl Pts',(-4.64999999999999,80.9210526315789,8.05403625519526));
#25742=CARTESIAN_POINT('Ctrl Pts',(-6.80807251039055,81.1184210526315,6.80807251039055));
#25743=CARTESIAN_POINT('Ctrl Pts',(-8.05403625519526,81.3157894736842,4.65));
#25744=CARTESIAN_POINT('Ctrl Pts',(-9.29999999999998,81.5131578947368,2.49192748960944));
#25745=CARTESIAN_POINT('Ctrl Pts',(-9.29999999999998,81.7105263157895,5.69460761604603E-16));
#25746=CARTESIAN_POINT('Ctrl Pts',(-9.29999999999998,81.9078947368421,-2.49192748960943));
#25747=CARTESIAN_POINT('Ctrl Pts',(-8.05403625519526,82.1052631578948,-4.64999999999998));
#25748=CARTESIAN_POINT('Ctrl Pts',(-6.80807251039055,82.3026315789473,-6.80807251039055));
#25749=CARTESIAN_POINT('Ctrl Pts',(-4.64999999999999,82.5,-8.05403625519526));
#25750=CARTESIAN_POINT('Ctrl Pts',(-2.49192748960944,82.6973684210527,-9.29999999999998));
#25751=CARTESIAN_POINT('Ctrl Pts',(-1.13892152320618E-15,82.8947368421053,
-9.29999999999998));
#25752=CARTESIAN_POINT('Ctrl Pts',(2.49192748960943,83.0921052631579,-9.29999999999999));
#25753=CARTESIAN_POINT('Ctrl Pts',(4.64999999999999,83.2894736842105,-8.05403625519526));
#25754=CARTESIAN_POINT('Ctrl Pts',(6.80807251039055,83.4868421052631,-6.80807251039056));
#25755=CARTESIAN_POINT('Ctrl Pts',(8.05403625519526,83.6842105263158,-4.64999999999999));
#25756=CARTESIAN_POINT('Ctrl Pts',(9.29999999999998,83.8815789473684,-2.49192748960945));
#25757=CARTESIAN_POINT('Ctrl Pts',(9.29999999999998,84.078947368421,-1.70838228480937E-15));
#25758=CARTESIAN_POINT('Ctrl Pts',(9.29999999999998,84.2763157894737,2.49192748960943));
#25759=CARTESIAN_POINT('Ctrl Pts',(8.05403625519526,84.4736842105263,4.64999999999998));
#25760=CARTESIAN_POINT('Ctrl Pts',(6.80807251039055,84.6710526315789,6.80807251039055));
#25761=CARTESIAN_POINT('Ctrl Pts',(4.64999999999999,84.8684210526316,8.05403625519526));
#25762=CARTESIAN_POINT('Ctrl Pts',(2.49192748960944,85.0657894736842,9.29999999999998));
#25763=CARTESIAN_POINT('Ctrl Pts',(9.87616875481775E-28,85.2631578947368,
9.29999999999998));
#25764=CARTESIAN_POINT('Ctrl Pts',(-2.49192748960943,85.4605263157894,9.29999999999998));
#25765=CARTESIAN_POINT('Ctrl Pts',(-4.64999999999999,85.6578947368421,8.05403625519527));
#25766=CARTESIAN_POINT('Ctrl Pts',(-6.80807251039055,85.8552631578947,6.80807251039054));
#25767=CARTESIAN_POINT('Ctrl Pts',(-8.05403625519526,86.0526315789474,4.65));
#25768=CARTESIAN_POINT('Ctrl Pts',(-9.29999999999998,86.25,2.49192748960944));
#25769=CARTESIAN_POINT('Ctrl Pts',(-9.29999999999998,86.4473684210526,5.6946076160411E-16));
#25770=CARTESIAN_POINT('Ctrl Pts',(-9.29999999999998,86.6447368421052,-2.49192748960943));
#25771=CARTESIAN_POINT('Ctrl Pts',(-8.05403625519526,86.8421052631579,-4.64999999999998));
#25772=CARTESIAN_POINT('Ctrl Pts',(-6.80807251039055,87.0394736842105,-6.80807251039055));
#25773=CARTESIAN_POINT('Ctrl Pts',(-4.64999999999999,87.2368421052631,-8.05403625519526));
#25774=CARTESIAN_POINT('Ctrl Pts',(-2.49192748960944,87.4342105263158,-9.29999999999998));
#25775=CARTESIAN_POINT('Ctrl Pts',(-1.13892152320613E-15,87.6315789473684,
-9.29999999999997));
#25776=CARTESIAN_POINT('Ctrl Pts',(2.49192748960943,87.828947368421,-9.29999999999998));
#25777=CARTESIAN_POINT('Ctrl Pts',(4.64999999999999,88.0263157894737,-8.05403625519526));
#25778=CARTESIAN_POINT('Ctrl Pts',(6.80807251039055,88.2236842105263,-6.80807251039055));
#25779=CARTESIAN_POINT('Ctrl Pts',(8.05403625519526,88.4210526315789,-4.64999999999999));
#25780=CARTESIAN_POINT('Ctrl Pts',(9.29999999999998,88.6184210526315,-2.49192748960944));
#25781=CARTESIAN_POINT('Ctrl Pts',(9.29999999999998,88.8157894736842,-1.70838228480927E-15));
#25782=CARTESIAN_POINT('Ctrl Pts',(9.29999999999998,89.0131578947368,2.49192748960943));
#25783=CARTESIAN_POINT('Ctrl Pts',(8.05403625519526,89.2105263157894,4.64999999999999));
#25784=CARTESIAN_POINT('Ctrl Pts',(6.80807251039055,89.4078947368421,6.80807251039054));
#25785=CARTESIAN_POINT('Ctrl Pts',(4.64999999999999,89.6052631578947,8.05403625519527));
#25786=CARTESIAN_POINT('Ctrl Pts',(2.49192748960944,89.8026315789473,9.29999999999996));
#25787=CARTESIAN_POINT('Ctrl Pts',(1.03537993810258E-27,90.,9.29999999999998));
#25788=CARTESIAN_POINT('Ctrl Pts',(6.93334779979405E-30,-4.00000000000002,
9.29999999999999));
#25789=CARTESIAN_POINT('Ctrl Pts',(-2.49192748960944,-3.80263157894737,
9.29999999999998));
#25790=CARTESIAN_POINT('Ctrl Pts',(-4.64999999999999,-3.60526315789474,
8.05403625519527));
#25791=CARTESIAN_POINT('Ctrl Pts',(-6.80807251039054,-3.40789473684211,
6.80807251039054));
#25792=CARTESIAN_POINT('Ctrl Pts',(-8.05403625519527,-3.21052631578946,
4.64999999999999));
#25793=CARTESIAN_POINT('Ctrl Pts',(-9.29999999999998,-3.01315789473685,
2.49192748960944));
#25794=CARTESIAN_POINT('Ctrl Pts',(-9.29999999999999,-2.81578947368422,
5.69460761603572E-16));
#25795=CARTESIAN_POINT('Ctrl Pts',(-9.29999999999998,-2.61842105263159,
-2.49192748960943));
#25796=CARTESIAN_POINT('Ctrl Pts',(-8.05403625519527,-2.42105263157898,
-4.64999999999999));
#25797=CARTESIAN_POINT('Ctrl Pts',(-6.80807251039054,-2.22368421052628,
-6.80807251039054));
#25798=CARTESIAN_POINT('Ctrl Pts',(-4.65,-2.02631578947365,-8.05403625519526));
#25799=CARTESIAN_POINT('Ctrl Pts',(-2.49192748960944,-1.82894736842106,
-9.29999999999998));
#25800=CARTESIAN_POINT('Ctrl Pts',(-1.13892152320711E-15,-1.63157894736841,
-9.29999999999999));
#25801=CARTESIAN_POINT('Ctrl Pts',(2.49192748960943,-1.43421052631576,-9.29999999999999));
#25802=CARTESIAN_POINT('Ctrl Pts',(4.64999999999999,-1.23684210526313,-8.05403625519527));
#25803=CARTESIAN_POINT('Ctrl Pts',(6.80807251039054,-1.0394736842105,-6.80807251039055));
#25804=CARTESIAN_POINT('Ctrl Pts',(8.05403625519526,-0.842105263157894,
-4.65));
#25805=CARTESIAN_POINT('Ctrl Pts',(9.29999999999998,-0.644736842105277,
-2.49192748960945));
#25806=CARTESIAN_POINT('Ctrl Pts',(9.29999999999999,-0.447368421052613,
-1.70838228481055E-15));
#25807=CARTESIAN_POINT('Ctrl Pts',(9.29999999999999,-0.249999999999972,
2.49192748960943));
#25808=CARTESIAN_POINT('Ctrl Pts',(8.05403625519527,-0.0526315789473736,
4.64999999999998));
#25809=CARTESIAN_POINT('Ctrl Pts',(6.80807251039055,0.144736842105247,6.80807251039054));
#25810=CARTESIAN_POINT('Ctrl Pts',(4.65,0.342105263157866,8.05403625519526));
#25811=CARTESIAN_POINT('Ctrl Pts',(2.49192748960945,0.539473684210509,9.29999999999998));
#25812=CARTESIAN_POINT('Ctrl Pts',(6.24001301981464E-29,0.736842105263147,
9.29999999999999));
#25813=CARTESIAN_POINT('Ctrl Pts',(-2.49192748960944,0.934210526315771,
9.29999999999998));
#25814=CARTESIAN_POINT('Ctrl Pts',(-4.64999999999999,1.13157894736839,8.05403625519527));
#25815=CARTESIAN_POINT('Ctrl Pts',(-6.80807251039054,1.32894736842103,6.80807251039054));
#25816=CARTESIAN_POINT('Ctrl Pts',(-8.05403625519527,1.52631578947371,4.64999999999999));
#25817=CARTESIAN_POINT('Ctrl Pts',(-9.29999999999998,1.72368421052634,2.49192748960944));
#25818=CARTESIAN_POINT('Ctrl Pts',(-9.29999999999999,1.92105263157895,5.69460761603572E-16));
#25819=CARTESIAN_POINT('Ctrl Pts',(-9.29999999999998,2.11842105263156,-2.49192748960944));
#25820=CARTESIAN_POINT('Ctrl Pts',(-8.05403625519527,2.31578947368419,-4.64999999999999));
#25821=CARTESIAN_POINT('Ctrl Pts',(-6.80807251039054,2.51315789473686,-6.80807251039054));
#25822=CARTESIAN_POINT('Ctrl Pts',(-4.65,2.71052631578947,-8.05403625519526));
#25823=CARTESIAN_POINT('Ctrl Pts',(-2.49192748960944,2.90789473684212,-9.29999999999998));
#25824=CARTESIAN_POINT('Ctrl Pts',(-1.13892152320705E-15,3.10526315789475,
-9.29999999999998));
#25825=CARTESIAN_POINT('Ctrl Pts',(2.49192748960943,3.30263157894739,-9.29999999999999));
#25826=CARTESIAN_POINT('Ctrl Pts',(4.64999999999999,3.50000000000003,-8.05403625519526));
#25827=CARTESIAN_POINT('Ctrl Pts',(6.80807251039054,3.69736842105265,-6.80807251039055));
#25828=CARTESIAN_POINT('Ctrl Pts',(8.05403625519526,3.89473684210523,-4.65));
#25829=CARTESIAN_POINT('Ctrl Pts',(9.29999999999998,4.09210526315787,-2.49192748960944));
#25830=CARTESIAN_POINT('Ctrl Pts',(9.29999999999999,4.28947368421051,-1.7083822848107E-15));
#25831=CARTESIAN_POINT('Ctrl Pts',(9.29999999999999,4.48684210526317,2.49192748960943));
#25832=CARTESIAN_POINT('Ctrl Pts',(8.05403625519527,4.68421052631579,4.64999999999999));
#25833=CARTESIAN_POINT('Ctrl Pts',(6.80807251039055,4.88157894736839,6.80807251039054));
#25834=CARTESIAN_POINT('Ctrl Pts',(4.65,5.07894736842103,8.05403625519526));
#25835=CARTESIAN_POINT('Ctrl Pts',(2.49192748960945,5.27631578947365,9.29999999999998));
#25836=CARTESIAN_POINT('Ctrl Pts',(1.10933564796705E-28,5.47368421052631,
9.29999999999999));
#25837=CARTESIAN_POINT('Ctrl Pts',(-2.49192748960944,5.67105263157892,9.29999999999998));
#25838=CARTESIAN_POINT('Ctrl Pts',(-4.64999999999999,5.86842105263155,8.05403625519527));
#25839=CARTESIAN_POINT('Ctrl Pts',(-6.80807251039054,6.06578947368418,6.80807251039054));
#25840=CARTESIAN_POINT('Ctrl Pts',(-8.05403625519527,6.26315789473687,4.64999999999999));
#25841=CARTESIAN_POINT('Ctrl Pts',(-9.29999999999998,6.46052631578948,2.49192748960944));
#25842=CARTESIAN_POINT('Ctrl Pts',(-9.29999999999999,6.65789473684211,5.69460761603572E-16));
#25843=CARTESIAN_POINT('Ctrl Pts',(-9.29999999999998,6.85526315789475,-2.49192748960944));
#25844=CARTESIAN_POINT('Ctrl Pts',(-8.05403625519527,7.05263157894735,-4.64999999999999));
#25845=CARTESIAN_POINT('Ctrl Pts',(-6.80807251039054,7.25000000000001,-6.80807251039054));
#25846=CARTESIAN_POINT('Ctrl Pts',(-4.65,7.44736842105263,-8.05403625519526));
#25847=CARTESIAN_POINT('Ctrl Pts',(-2.49192748960944,7.64473684210527,-9.29999999999998));
#25848=CARTESIAN_POINT('Ctrl Pts',(-1.138921523207E-15,7.84210526315791,
-9.29999999999999));
#25849=CARTESIAN_POINT('Ctrl Pts',(2.49192748960943,8.03947368421053,-9.29999999999999));
#25850=CARTESIAN_POINT('Ctrl Pts',(4.64999999999999,8.23684210526315,-8.05403625519527));
#25851=CARTESIAN_POINT('Ctrl Pts',(6.80807251039054,8.43421052631579,-6.80807251039055));
#25852=CARTESIAN_POINT('Ctrl Pts',(8.05403625519526,8.63157894736839,-4.65));
#25853=CARTESIAN_POINT('Ctrl Pts',(9.29999999999998,8.82894736842105,-2.49192748960944));
#25854=CARTESIAN_POINT('Ctrl Pts',(9.29999999999999,9.02631578947367,-1.7083822848107E-15));
#25855=CARTESIAN_POINT('Ctrl Pts',(9.29999999999999,9.22368421052632,2.49192748960943));
#25856=CARTESIAN_POINT('Ctrl Pts',(8.05403625519527,9.42105263157895,4.64999999999998));
#25857=CARTESIAN_POINT('Ctrl Pts',(6.80807251039055,9.61842105263154,6.80807251039054));
#25858=CARTESIAN_POINT('Ctrl Pts',(4.65,9.81578947368419,8.05403625519527));
#25859=CARTESIAN_POINT('Ctrl Pts',(2.49192748960945,10.0131578947368,9.29999999999998));
#25860=CARTESIAN_POINT('Ctrl Pts',(1.60622557361895E-28,10.2105263157895,
9.29999999999999));
#25861=CARTESIAN_POINT('Ctrl Pts',(-2.49192748960944,10.4078947368421,9.29999999999998));
#25862=CARTESIAN_POINT('Ctrl Pts',(-4.64999999999999,10.6052631578947,8.05403625519527));
#25863=CARTESIAN_POINT('Ctrl Pts',(-6.80807251039054,10.8026315789474,6.80807251039054));
#25864=CARTESIAN_POINT('Ctrl Pts',(-8.05403625519527,11.,4.64999999999999));
#25865=CARTESIAN_POINT('Ctrl Pts',(-9.29999999999998,11.1973684210526,2.49192748960944));
#25866=CARTESIAN_POINT('Ctrl Pts',(-9.29999999999999,11.3947368421053,5.69460761603572E-16));
#25867=CARTESIAN_POINT('Ctrl Pts',(-9.29999999999998,11.5921052631579,-2.49192748960944));
#25868=CARTESIAN_POINT('Ctrl Pts',(-8.05403625519527,11.7894736842105,-4.64999999999999));
#25869=CARTESIAN_POINT('Ctrl Pts',(-6.80807251039054,11.9868421052632,-6.80807251039054));
#25870=CARTESIAN_POINT('Ctrl Pts',(-4.65,12.1842105263158,-8.05403625519526));
#25871=CARTESIAN_POINT('Ctrl Pts',(-2.49192748960944,12.3815789473684,-9.29999999999998));
#25872=CARTESIAN_POINT('Ctrl Pts',(-1.13892152320695E-15,12.5789473684211,
-9.29999999999999));
#25873=CARTESIAN_POINT('Ctrl Pts',(2.49192748960943,12.7763157894737,-9.29999999999999));
#25874=CARTESIAN_POINT('Ctrl Pts',(4.64999999999999,12.9736842105263,-8.05403625519527));
#25875=CARTESIAN_POINT('Ctrl Pts',(6.80807251039054,13.171052631579,-6.80807251039055));
#25876=CARTESIAN_POINT('Ctrl Pts',(8.05403625519526,13.3684210526316,-4.65));
#25877=CARTESIAN_POINT('Ctrl Pts',(9.29999999999998,13.5657894736842,-2.49192748960944));
#25878=CARTESIAN_POINT('Ctrl Pts',(9.29999999999999,13.7631578947368,-1.7083822848107E-15));
#25879=CARTESIAN_POINT('Ctrl Pts',(9.29999999999999,13.9605263157895,2.49192748960943));
#25880=CARTESIAN_POINT('Ctrl Pts',(8.05403625519527,14.1578947368421,4.64999999999999));
#25881=CARTESIAN_POINT('Ctrl Pts',(6.80807251039055,14.3552631578947,6.80807251039054));
#25882=CARTESIAN_POINT('Ctrl Pts',(4.65,14.5526315789474,8.05403625519526));
#25883=CARTESIAN_POINT('Ctrl Pts',(2.49192748960945,14.75,9.29999999999998));
#25884=CARTESIAN_POINT('Ctrl Pts',(2.14933781793615E-28,14.9473684210526,
9.29999999999999));
#25885=CARTESIAN_POINT('Ctrl Pts',(-2.49192748960944,15.1447368421053,9.29999999999998));
#25886=CARTESIAN_POINT('Ctrl Pts',(-4.64999999999999,15.3421052631579,8.05403625519527));
#25887=CARTESIAN_POINT('Ctrl Pts',(-6.80807251039054,15.5394736842105,6.80807251039054));
#25888=CARTESIAN_POINT('Ctrl Pts',(-8.05403625519527,15.7368421052632,4.64999999999999));
#25889=CARTESIAN_POINT('Ctrl Pts',(-9.29999999999998,15.9342105263158,2.49192748960944));
#25890=CARTESIAN_POINT('Ctrl Pts',(-9.29999999999999,16.1315789473684,5.69460761603425E-16));
#25891=CARTESIAN_POINT('Ctrl Pts',(-9.29999999999998,16.328947368421,-2.49192748960944));
#25892=CARTESIAN_POINT('Ctrl Pts',(-8.05403625519527,16.5263157894737,-4.64999999999999));
#25893=CARTESIAN_POINT('Ctrl Pts',(-6.80807251039054,16.7236842105263,-6.80807251039054));
#25894=CARTESIAN_POINT('Ctrl Pts',(-4.65,16.921052631579,-8.05403625519526));
#25895=CARTESIAN_POINT('Ctrl Pts',(-2.49192748960944,17.1184210526316,-9.29999999999998));
#25896=CARTESIAN_POINT('Ctrl Pts',(-1.1389215232069E-15,17.3157894736842,
-9.29999999999998));
#25897=CARTESIAN_POINT('Ctrl Pts',(2.49192748960943,17.5131578947369,-9.29999999999999));
#25898=CARTESIAN_POINT('Ctrl Pts',(4.64999999999999,17.7105263157895,-8.05403625519527));
#25899=CARTESIAN_POINT('Ctrl Pts',(6.80807251039054,17.9078947368421,-6.80807251039055));
#25900=CARTESIAN_POINT('Ctrl Pts',(8.05403625519526,18.1052631578947,-4.65));
#25901=CARTESIAN_POINT('Ctrl Pts',(9.29999999999998,18.3026315789473,-2.49192748960944));
#25902=CARTESIAN_POINT('Ctrl Pts',(9.29999999999999,18.5,-1.70838228481055E-15));
#25903=CARTESIAN_POINT('Ctrl Pts',(9.29999999999999,18.6973684210526,2.49192748960943));
#25904=CARTESIAN_POINT('Ctrl Pts',(8.05403625519527,18.8947368421053,4.64999999999998));
#25905=CARTESIAN_POINT('Ctrl Pts',(6.80807251039055,19.0921052631579,6.80807251039054));
#25906=CARTESIAN_POINT('Ctrl Pts',(4.65,19.2894736842105,8.05403625519526));
#25907=CARTESIAN_POINT('Ctrl Pts',(2.49192748960945,19.4868421052631,9.29999999999998));
#25908=CARTESIAN_POINT('Ctrl Pts',(2.70400564191968E-28,19.6842105263158,
9.29999999999999));
#25909=CARTESIAN_POINT('Ctrl Pts',(-2.49192748960944,19.8815789473684,9.29999999999998));
#25910=CARTESIAN_POINT('Ctrl Pts',(-4.64999999999999,20.078947368421,8.05403625519527));
#25911=CARTESIAN_POINT('Ctrl Pts',(-6.80807251039054,20.2763157894737,6.80807251039055));
#25912=CARTESIAN_POINT('Ctrl Pts',(-8.05403625519527,20.4736842105263,4.64999999999999));
#25913=CARTESIAN_POINT('Ctrl Pts',(-9.29999999999998,20.671052631579,2.49192748960944));
#25914=CARTESIAN_POINT('Ctrl Pts',(-9.29999999999999,20.8684210526316,5.69460761603572E-16));
#25915=CARTESIAN_POINT('Ctrl Pts',(-9.29999999999998,21.0657894736842,-2.49192748960943));
#25916=CARTESIAN_POINT('Ctrl Pts',(-8.05403625519527,21.2631578947368,-4.64999999999999));
#25917=CARTESIAN_POINT('Ctrl Pts',(-6.80807251039054,21.4605263157895,-6.80807251039054));
#25918=CARTESIAN_POINT('Ctrl Pts',(-4.65,21.6578947368421,-8.05403625519526));
#25919=CARTESIAN_POINT('Ctrl Pts',(-2.49192748960944,21.8552631578947,-9.29999999999998));
#25920=CARTESIAN_POINT('Ctrl Pts',(-1.13892152320684E-15,22.0526315789474,
-9.29999999999999));
#25921=CARTESIAN_POINT('Ctrl Pts',(2.49192748960943,22.25,-9.29999999999999));
#25922=CARTESIAN_POINT('Ctrl Pts',(4.64999999999999,22.4473684210526,-8.05403625519526));
#25923=CARTESIAN_POINT('Ctrl Pts',(6.80807251039054,22.6447368421053,-6.80807251039055));
#25924=CARTESIAN_POINT('Ctrl Pts',(8.05403625519526,22.8421052631579,-4.65));
#25925=CARTESIAN_POINT('Ctrl Pts',(9.29999999999998,23.0394736842105,-2.49192748960944));
#25926=CARTESIAN_POINT('Ctrl Pts',(9.29999999999999,23.2368421052632,-1.70838228481055E-15));
#25927=CARTESIAN_POINT('Ctrl Pts',(9.29999999999999,23.4342105263158,2.49192748960943));
#25928=CARTESIAN_POINT('Ctrl Pts',(8.05403625519527,23.6315789473684,4.64999999999998));
#25929=CARTESIAN_POINT('Ctrl Pts',(6.80807251039055,23.828947368421,6.80807251039054));
#25930=CARTESIAN_POINT('Ctrl Pts',(4.65,24.0263157894736,8.05403625519526));
#25931=CARTESIAN_POINT('Ctrl Pts',(2.49192748960945,24.2236842105263,9.29999999999998));
#25932=CARTESIAN_POINT('Ctrl Pts',(3.16622882857262E-28,24.4210526315789,
9.29999999999999));
#25933=CARTESIAN_POINT('Ctrl Pts',(-2.49192748960944,24.6184210526316,9.29999999999998));
#25934=CARTESIAN_POINT('Ctrl Pts',(-4.64999999999999,24.8157894736842,8.05403625519527));
#25935=CARTESIAN_POINT('Ctrl Pts',(-6.80807251039054,25.0131578947368,6.80807251039054));
#25936=CARTESIAN_POINT('Ctrl Pts',(-8.05403625519527,25.2105263157895,4.64999999999999));
#25937=CARTESIAN_POINT('Ctrl Pts',(-9.29999999999998,25.4078947368421,2.49192748960944));
#25938=CARTESIAN_POINT('Ctrl Pts',(-9.29999999999999,25.6052631578947,5.69460761603572E-16));
#25939=CARTESIAN_POINT('Ctrl Pts',(-9.29999999999998,25.8026315789474,-2.49192748960943));
#25940=CARTESIAN_POINT('Ctrl Pts',(-8.05403625519527,26.,-4.64999999999999));
#25941=CARTESIAN_POINT('Ctrl Pts',(-6.80807251039054,26.1973684210526,-6.80807251039054));
#25942=CARTESIAN_POINT('Ctrl Pts',(-4.65,26.3947368421053,-8.05403625519526));
#25943=CARTESIAN_POINT('Ctrl Pts',(-2.49192748960944,26.5921052631579,-9.29999999999998));
#25944=CARTESIAN_POINT('Ctrl Pts',(-1.13892152320679E-15,26.7894736842105,
-9.29999999999999));
#25945=CARTESIAN_POINT('Ctrl Pts',(2.49192748960943,26.9868421052632,-9.29999999999999));
#25946=CARTESIAN_POINT('Ctrl Pts',(4.64999999999999,27.1842105263158,-8.05403625519527));
#25947=CARTESIAN_POINT('Ctrl Pts',(6.80807251039054,27.3815789473685,-6.80807251039055));
#25948=CARTESIAN_POINT('Ctrl Pts',(8.05403625519526,27.578947368421,-4.65));
#25949=CARTESIAN_POINT('Ctrl Pts',(9.29999999999998,27.7763157894737,-2.49192748960944));
#25950=CARTESIAN_POINT('Ctrl Pts',(9.29999999999999,27.9736842105263,-1.70838228481055E-15));
#25951=CARTESIAN_POINT('Ctrl Pts',(9.29999999999999,28.1710526315789,2.49192748960943));
#25952=CARTESIAN_POINT('Ctrl Pts',(8.05403625519527,28.3684210526316,4.64999999999999));
#25953=CARTESIAN_POINT('Ctrl Pts',(6.80807251039055,28.5657894736842,6.80807251039054));
#25954=CARTESIAN_POINT('Ctrl Pts',(4.65,28.7631578947368,8.05403625519526));
#25955=CARTESIAN_POINT('Ctrl Pts',(2.49192748960945,28.9605263157895,9.29999999999998));
#25956=CARTESIAN_POINT('Ctrl Pts',(3.67467433389085E-28,29.1578947368421,
9.29999999999999));
#25957=CARTESIAN_POINT('Ctrl Pts',(-2.49192748960944,29.3552631578947,9.29999999999998));
#25958=CARTESIAN_POINT('Ctrl Pts',(-4.64999999999999,29.5526315789473,8.05403625519527));
#25959=CARTESIAN_POINT('Ctrl Pts',(-6.80807251039054,29.7499999999999,6.80807251039054));
#25960=CARTESIAN_POINT('Ctrl Pts',(-8.05403625519527,29.9473684210527,4.64999999999999));
#25961=CARTESIAN_POINT('Ctrl Pts',(-9.29999999999998,30.1447368421053,2.49192748960944));
#25962=CARTESIAN_POINT('Ctrl Pts',(-9.29999999999999,30.3421052631579,5.69460761603572E-16));
#25963=CARTESIAN_POINT('Ctrl Pts',(-9.29999999999998,30.5394736842105,-2.49192748960943));
#25964=CARTESIAN_POINT('Ctrl Pts',(-8.05403625519527,30.7368421052631,-4.64999999999999));
#25965=CARTESIAN_POINT('Ctrl Pts',(-6.80807251039054,30.9342105263159,-6.80807251039054));
#25966=CARTESIAN_POINT('Ctrl Pts',(-4.65,31.1315789473685,-8.05403625519526));
#25967=CARTESIAN_POINT('Ctrl Pts',(-2.49192748960944,31.3289473684211,-9.29999999999998));
#25968=CARTESIAN_POINT('Ctrl Pts',(-1.13892152320674E-15,31.5263157894737,
-9.29999999999999));
#25969=CARTESIAN_POINT('Ctrl Pts',(2.49192748960943,31.7236842105263,-9.29999999999999));
#25970=CARTESIAN_POINT('Ctrl Pts',(4.64999999999999,31.921052631579,-8.05403625519527));
#25971=CARTESIAN_POINT('Ctrl Pts',(6.80807251039054,32.1184210526316,-6.80807251039055));
#25972=CARTESIAN_POINT('Ctrl Pts',(8.05403625519526,32.3157894736842,-4.65));
#25973=CARTESIAN_POINT('Ctrl Pts',(9.29999999999998,32.5131578947368,-2.49192748960945));
#25974=CARTESIAN_POINT('Ctrl Pts',(9.29999999999999,32.7105263157895,-1.7083822848107E-15));
#25975=CARTESIAN_POINT('Ctrl Pts',(9.29999999999999,32.9078947368421,2.49192748960943));
#25976=CARTESIAN_POINT('Ctrl Pts',(8.05403625519527,33.1052631578947,4.64999999999998));
#25977=CARTESIAN_POINT('Ctrl Pts',(6.80807251039055,33.3026315789473,6.80807251039054));
#25978=CARTESIAN_POINT('Ctrl Pts',(4.65,33.5,8.05403625519526));
#25979=CARTESIAN_POINT('Ctrl Pts',(2.49192748960945,33.6973684210526,9.29999999999998));
#25980=CARTESIAN_POINT('Ctrl Pts',(4.22934215787437E-28,33.8947368421052,
9.29999999999999));
#25981=CARTESIAN_POINT('Ctrl Pts',(-2.49192748960944,34.0921052631579,9.29999999999998));
#25982=CARTESIAN_POINT('Ctrl Pts',(-4.64999999999999,34.2894736842105,8.05403625519527));
#25983=CARTESIAN_POINT('Ctrl Pts',(-6.80807251039054,34.4868421052631,6.80807251039054));
#25984=CARTESIAN_POINT('Ctrl Pts',(-8.05403625519527,34.6842105263158,4.64999999999999));
#25985=CARTESIAN_POINT('Ctrl Pts',(-9.29999999999998,34.8815789473684,2.49192748960944));
#25986=CARTESIAN_POINT('Ctrl Pts',(-9.29999999999999,35.078947368421,5.69460761603572E-16));
#25987=CARTESIAN_POINT('Ctrl Pts',(-9.29999999999998,35.2763157894737,-2.49192748960943));
#25988=CARTESIAN_POINT('Ctrl Pts',(-8.05403625519527,35.4736842105263,-4.64999999999999));
#25989=CARTESIAN_POINT('Ctrl Pts',(-6.80807251039054,35.671052631579,-6.80807251039054));
#25990=CARTESIAN_POINT('Ctrl Pts',(-4.65,35.8684210526316,-8.05403625519526));
#25991=CARTESIAN_POINT('Ctrl Pts',(-2.49192748960944,36.0657894736842,-9.29999999999998));
#25992=CARTESIAN_POINT('Ctrl Pts',(-1.13892152320669E-15,36.2631578947368,
-9.29999999999998));
#25993=CARTESIAN_POINT('Ctrl Pts',(2.49192748960943,36.4605263157895,-9.29999999999999));
#25994=CARTESIAN_POINT('Ctrl Pts',(4.64999999999999,36.6578947368421,-8.05403625519526));
#25995=CARTESIAN_POINT('Ctrl Pts',(6.80807251039054,36.8552631578947,-6.80807251039055));
#25996=CARTESIAN_POINT('Ctrl Pts',(8.05403625519526,37.0526315789473,-4.65));
#25997=CARTESIAN_POINT('Ctrl Pts',(9.29999999999998,37.25,-2.49192748960945));
#25998=CARTESIAN_POINT('Ctrl Pts',(9.29999999999999,37.4473684210526,-1.70838228481055E-15));
#25999=CARTESIAN_POINT('Ctrl Pts',(9.29999999999999,37.6447368421053,2.49192748960943));
#26000=CARTESIAN_POINT('Ctrl Pts',(8.05403625519527,37.8421052631579,4.64999999999999));
#26001=CARTESIAN_POINT('Ctrl Pts',(6.80807251039055,38.0394736842105,6.80807251039054));
#26002=CARTESIAN_POINT('Ctrl Pts',(4.65,38.2368421052631,8.05403625519526));
#26003=CARTESIAN_POINT('Ctrl Pts',(2.49192748960945,38.4342105263158,9.29999999999998));
#26004=CARTESIAN_POINT('Ctrl Pts',(4.78400998185789E-28,38.6315789473684,
9.29999999999999));
#26005=CARTESIAN_POINT('Ctrl Pts',(-2.49192748960944,38.828947368421,9.29999999999998));
#26006=CARTESIAN_POINT('Ctrl Pts',(-4.64999999999999,39.0263157894736,8.05403625519527));
#26007=CARTESIAN_POINT('Ctrl Pts',(-6.80807251039054,39.2236842105262,6.80807251039054));
#26008=CARTESIAN_POINT('Ctrl Pts',(-8.05403625519527,39.421052631579,4.64999999999999));
#26009=CARTESIAN_POINT('Ctrl Pts',(-9.29999999999998,39.6184210526316,2.49192748960944));
#26010=CARTESIAN_POINT('Ctrl Pts',(-9.29999999999999,39.8157894736842,5.69460761603572E-16));
#26011=CARTESIAN_POINT('Ctrl Pts',(-9.29999999999998,40.0131578947368,-2.49192748960943));
#26012=CARTESIAN_POINT('Ctrl Pts',(-8.05403625519527,40.2105263157895,-4.64999999999999));
#26013=CARTESIAN_POINT('Ctrl Pts',(-6.80807251039054,40.4078947368421,-6.80807251039054));
#26014=CARTESIAN_POINT('Ctrl Pts',(-4.65,40.6052631578947,-8.05403625519526));
#26015=CARTESIAN_POINT('Ctrl Pts',(-2.49192748960944,40.8026315789474,-9.29999999999998));
#26016=CARTESIAN_POINT('Ctrl Pts',(-1.13892152320664E-15,41.,-9.29999999999999));
#26017=CARTESIAN_POINT('Ctrl Pts',(2.49192748960943,41.1973684210526,-9.29999999999999));
#26018=CARTESIAN_POINT('Ctrl Pts',(4.64999999999999,41.3947368421053,-8.05403625519527));
#26019=CARTESIAN_POINT('Ctrl Pts',(6.80807251039054,41.5921052631579,-6.80807251039055));
#26020=CARTESIAN_POINT('Ctrl Pts',(8.05403625519526,41.7894736842105,-4.65));
#26021=CARTESIAN_POINT('Ctrl Pts',(9.29999999999998,41.9868421052632,-2.49192748960945));
#26022=CARTESIAN_POINT('Ctrl Pts',(9.29999999999999,42.1842105263158,-1.70838228481055E-15));
#26023=CARTESIAN_POINT('Ctrl Pts',(9.29999999999999,42.3815789473684,2.49192748960943));
#26024=CARTESIAN_POINT('Ctrl Pts',(8.05403625519527,42.5789473684211,4.64999999999998));
#26025=CARTESIAN_POINT('Ctrl Pts',(6.80807251039055,42.7763157894736,6.80807251039054));
#26026=CARTESIAN_POINT('Ctrl Pts',(4.65,42.9736842105263,8.05403625519527));
#26027=CARTESIAN_POINT('Ctrl Pts',(2.49192748960945,43.1710526315789,9.29999999999998));
#26028=CARTESIAN_POINT('Ctrl Pts',(5.26934432784348E-28,43.3684210526316,
9.29999999999999));
#26029=CARTESIAN_POINT('Ctrl Pts',(-2.49192748960944,43.5657894736842,9.29999999999998));
#26030=CARTESIAN_POINT('Ctrl Pts',(-4.64999999999999,43.7631578947368,8.05403625519527));
#26031=CARTESIAN_POINT('Ctrl Pts',(-6.80807251039054,43.9605263157895,6.80807251039054));
#26032=CARTESIAN_POINT('Ctrl Pts',(-8.05403625519527,44.1578947368421,4.64999999999999));
#26033=CARTESIAN_POINT('Ctrl Pts',(-9.29999999999998,44.3552631578947,2.49192748960944));
#26034=CARTESIAN_POINT('Ctrl Pts',(-9.29999999999999,44.5526315789474,5.6946076160372E-16));
#26035=CARTESIAN_POINT('Ctrl Pts',(-9.29999999999998,44.75,-2.49192748960944));
#26036=CARTESIAN_POINT('Ctrl Pts',(-8.05403625519527,44.9473684210526,-4.64999999999999));
#26037=CARTESIAN_POINT('Ctrl Pts',(-6.80807251039054,45.1447368421053,-6.80807251039054));
#26038=CARTESIAN_POINT('Ctrl Pts',(-4.65,45.3421052631579,-8.05403625519526));
#26039=CARTESIAN_POINT('Ctrl Pts',(-2.49192748960944,45.5394736842105,-9.29999999999998));
#26040=CARTESIAN_POINT('Ctrl Pts',(-1.13892152320659E-15,45.7368421052632,
-9.29999999999999));
#26041=CARTESIAN_POINT('Ctrl Pts',(2.49192748960943,45.9342105263158,-9.29999999999999));
#26042=CARTESIAN_POINT('Ctrl Pts',(4.64999999999999,46.1315789473684,-8.05403625519527));
#26043=CARTESIAN_POINT('Ctrl Pts',(6.80807251039054,46.328947368421,-6.80807251039055));
#26044=CARTESIAN_POINT('Ctrl Pts',(8.05403625519526,46.5263157894737,-4.65));
#26045=CARTESIAN_POINT('Ctrl Pts',(9.29999999999998,46.7236842105263,-2.49192748960944));
#26046=CARTESIAN_POINT('Ctrl Pts',(9.29999999999999,46.9210526315789,-1.70838228481055E-15));
#26047=CARTESIAN_POINT('Ctrl Pts',(9.29999999999999,47.1184210526316,2.49192748960943));
#26048=CARTESIAN_POINT('Ctrl Pts',(8.05403625519527,47.3157894736843,4.64999999999999));
#26049=CARTESIAN_POINT('Ctrl Pts',(6.80807251039055,47.5131578947368,6.80807251039054));
#26050=CARTESIAN_POINT('Ctrl Pts',(4.65,47.7105263157895,8.05403625519526));
#26051=CARTESIAN_POINT('Ctrl Pts',(2.49192748960945,47.9078947368421,9.29999999999998));
#26052=CARTESIAN_POINT('Ctrl Pts',(5.75467867382906E-28,48.1052631578947,
9.29999999999999));
#26053=CARTESIAN_POINT('Ctrl Pts',(-2.49192748960944,48.3026315789473,9.29999999999998));
#26054=CARTESIAN_POINT('Ctrl Pts',(-4.64999999999999,48.5,8.05403625519527));
#26055=CARTESIAN_POINT('Ctrl Pts',(-6.80807251039054,48.6973684210526,6.80807251039054));
#26056=CARTESIAN_POINT('Ctrl Pts',(-8.05403625519527,48.8947368421053,4.64999999999999));
#26057=CARTESIAN_POINT('Ctrl Pts',(-9.29999999999998,49.0921052631579,2.49192748960944));
#26058=CARTESIAN_POINT('Ctrl Pts',(-9.29999999999999,49.2894736842105,5.69460761603572E-16));
#26059=CARTESIAN_POINT('Ctrl Pts',(-9.29999999999998,49.4868421052631,-2.49192748960944));
#26060=CARTESIAN_POINT('Ctrl Pts',(-8.05403625519527,49.6842105263157,-4.64999999999999));
#26061=CARTESIAN_POINT('Ctrl Pts',(-6.80807251039054,49.8815789473684,-6.80807251039054));
#26062=CARTESIAN_POINT('Ctrl Pts',(-4.65,50.0789473684211,-8.05403625519526));
#26063=CARTESIAN_POINT('Ctrl Pts',(-2.49192748960944,50.2763157894737,-9.29999999999998));
#26064=CARTESIAN_POINT('Ctrl Pts',(-1.13892152320653E-15,50.4736842105263,
-9.29999999999998));
#26065=CARTESIAN_POINT('Ctrl Pts',(2.49192748960943,50.671052631579,-9.29999999999999));
#26066=CARTESIAN_POINT('Ctrl Pts',(4.64999999999999,50.8684210526316,-8.05403625519527));
#26067=CARTESIAN_POINT('Ctrl Pts',(6.80807251039054,51.0657894736843,-6.80807251039055));
#26068=CARTESIAN_POINT('Ctrl Pts',(8.05403625519526,51.2631578947368,-4.65));
#26069=CARTESIAN_POINT('Ctrl Pts',(9.29999999999998,51.4605263157895,-2.49192748960944));
#26070=CARTESIAN_POINT('Ctrl Pts',(9.29999999999999,51.6578947368421,-1.70838228481055E-15));
#26071=CARTESIAN_POINT('Ctrl Pts',(9.29999999999999,51.8552631578948,2.49192748960943));
#26072=CARTESIAN_POINT('Ctrl Pts',(8.05403625519527,52.0526315789474,4.64999999999998));
#26073=CARTESIAN_POINT('Ctrl Pts',(6.80807251039055,52.2499999999999,6.80807251039053));
#26074=CARTESIAN_POINT('Ctrl Pts',(4.65,52.4473684210526,8.05403625519526));
#26075=CARTESIAN_POINT('Ctrl Pts',(2.49192748960945,52.6447368421052,9.29999999999998));
#26076=CARTESIAN_POINT('Ctrl Pts',(6.30934649781258E-28,52.8421052631579,
9.29999999999999));
#26077=CARTESIAN_POINT('Ctrl Pts',(-2.49192748960944,53.0394736842105,9.29999999999999));
#26078=CARTESIAN_POINT('Ctrl Pts',(-4.64999999999999,53.2368421052632,8.05403625519527));
#26079=CARTESIAN_POINT('Ctrl Pts',(-6.80807251039054,53.4342105263158,6.80807251039055));
#26080=CARTESIAN_POINT('Ctrl Pts',(-8.05403625519527,53.6315789473684,4.64999999999999));
#26081=CARTESIAN_POINT('Ctrl Pts',(-9.29999999999998,53.8289473684211,2.49192748960944));
#26082=CARTESIAN_POINT('Ctrl Pts',(-9.29999999999999,54.0263157894737,5.69460761603572E-16));
#26083=CARTESIAN_POINT('Ctrl Pts',(-9.29999999999998,54.2236842105263,-2.49192748960944));
#26084=CARTESIAN_POINT('Ctrl Pts',(-8.05403625519527,54.4210526315789,-4.64999999999999));
#26085=CARTESIAN_POINT('Ctrl Pts',(-6.80807251039054,54.6184210526316,-6.80807251039054));
#26086=CARTESIAN_POINT('Ctrl Pts',(-4.65,54.8157894736842,-8.05403625519526));
#26087=CARTESIAN_POINT('Ctrl Pts',(-2.49192748960944,55.0131578947369,-9.29999999999998));
#26088=CARTESIAN_POINT('Ctrl Pts',(-1.13892152320648E-15,55.2105263157895,
-9.29999999999999));
#26089=CARTESIAN_POINT('Ctrl Pts',(2.49192748960943,55.4078947368421,-9.29999999999999));
#26090=CARTESIAN_POINT('Ctrl Pts',(4.64999999999999,55.6052631578947,-8.05403625519527));
#26091=CARTESIAN_POINT('Ctrl Pts',(6.80807251039054,55.8026315789474,-6.80807251039055));
#26092=CARTESIAN_POINT('Ctrl Pts',(8.05403625519526,55.9999999999999,-4.65));
#26093=CARTESIAN_POINT('Ctrl Pts',(9.29999999999998,56.1973684210526,-2.49192748960944));
#26094=CARTESIAN_POINT('Ctrl Pts',(9.29999999999999,56.3947368421052,-1.7083822848107E-15));
#26095=CARTESIAN_POINT('Ctrl Pts',(9.29999999999999,56.5921052631579,2.49192748960943));
#26096=CARTESIAN_POINT('Ctrl Pts',(8.05403625519527,56.7894736842106,4.64999999999998));
#26097=CARTESIAN_POINT('Ctrl Pts',(6.80807251039055,56.9868421052631,6.80807251039054));
#26098=CARTESIAN_POINT('Ctrl Pts',(4.65,57.1842105263158,8.05403625519526));
#26099=CARTESIAN_POINT('Ctrl Pts',(2.49192748960945,57.3815789473684,9.29999999999998));
#26100=CARTESIAN_POINT('Ctrl Pts',(6.73690294546655E-28,57.578947368421,
9.29999999999999));
#26101=CARTESIAN_POINT('Ctrl Pts',(-2.49192748960944,57.7763157894737,9.29999999999998));
#26102=CARTESIAN_POINT('Ctrl Pts',(-4.64999999999999,57.9736842105263,8.05403625519527));
#26103=CARTESIAN_POINT('Ctrl Pts',(-6.80807251039054,58.1710526315789,6.80807251039054));
#26104=CARTESIAN_POINT('Ctrl Pts',(-8.05403625519527,58.3684210526316,4.64999999999999));
#26105=CARTESIAN_POINT('Ctrl Pts',(-9.29999999999998,58.5657894736842,2.49192748960944));
#26106=CARTESIAN_POINT('Ctrl Pts',(-9.29999999999999,58.7631578947368,5.69460761603572E-16));
#26107=CARTESIAN_POINT('Ctrl Pts',(-9.29999999999998,58.9605263157895,-2.49192748960944));
#26108=CARTESIAN_POINT('Ctrl Pts',(-8.05403625519527,59.157894736842,-4.64999999999999));
#26109=CARTESIAN_POINT('Ctrl Pts',(-6.80807251039054,59.3552631578947,-6.80807251039054));
#26110=CARTESIAN_POINT('Ctrl Pts',(-4.65,59.5526315789473,-8.05403625519526));
#26111=CARTESIAN_POINT('Ctrl Pts',(-2.49192748960944,59.75,-9.29999999999998));
#26112=CARTESIAN_POINT('Ctrl Pts',(-1.13892152320643E-15,59.9473684210526,
-9.29999999999999));
#26113=CARTESIAN_POINT('Ctrl Pts',(2.49192748960943,60.1447368421053,-9.29999999999999));
#26114=CARTESIAN_POINT('Ctrl Pts',(4.64999999999999,60.3421052631579,-8.05403625519527));
#26115=CARTESIAN_POINT('Ctrl Pts',(6.80807251039054,60.5394736842106,-6.80807251039055));
#26116=CARTESIAN_POINT('Ctrl Pts',(8.05403625519526,60.7368421052631,-4.65));
#26117=CARTESIAN_POINT('Ctrl Pts',(9.29999999999998,60.9342105263158,-2.49192748960944));
#26118=CARTESIAN_POINT('Ctrl Pts',(9.29999999999999,61.1315789473684,-1.70838228481055E-15));
#26119=CARTESIAN_POINT('Ctrl Pts',(9.29999999999999,61.328947368421,2.49192748960943));
#26120=CARTESIAN_POINT('Ctrl Pts',(8.05403625519527,61.5263157894737,4.64999999999999));
#26121=CARTESIAN_POINT('Ctrl Pts',(6.80807251039055,61.7236842105263,6.80807251039054));
#26122=CARTESIAN_POINT('Ctrl Pts',(4.65,61.9210526315789,8.05403625519526));
#26123=CARTESIAN_POINT('Ctrl Pts',(2.49192748960945,62.1184210526316,9.29999999999998));
#26124=CARTESIAN_POINT('Ctrl Pts',(7.34934866778169E-28,62.3157894736842,
9.29999999999999));
#26125=CARTESIAN_POINT('Ctrl Pts',(-2.49192748960944,62.5131578947368,9.29999999999998));
#26126=CARTESIAN_POINT('Ctrl Pts',(-4.64999999999999,62.7105263157894,8.05403625519527));
#26127=CARTESIAN_POINT('Ctrl Pts',(-6.80807251039054,62.9078947368421,6.80807251039054));
#26128=CARTESIAN_POINT('Ctrl Pts',(-8.05403625519527,63.1052631578947,4.64999999999999));
#26129=CARTESIAN_POINT('Ctrl Pts',(-9.29999999999998,63.3026315789474,2.49192748960944));
#26130=CARTESIAN_POINT('Ctrl Pts',(-9.29999999999999,63.5,5.69460761603572E-16));
#26131=CARTESIAN_POINT('Ctrl Pts',(-9.29999999999998,63.6973684210526,-2.49192748960943));
#26132=CARTESIAN_POINT('Ctrl Pts',(-8.05403625519527,63.8947368421052,-4.64999999999999));
#26133=CARTESIAN_POINT('Ctrl Pts',(-6.80807251039054,64.092105263158,-6.80807251039054));
#26134=CARTESIAN_POINT('Ctrl Pts',(-4.65,64.2894736842105,-8.05403625519526));
#26135=CARTESIAN_POINT('Ctrl Pts',(-2.49192748960944,64.4868421052632,-9.29999999999998));
#26136=CARTESIAN_POINT('Ctrl Pts',(-1.13892152320638E-15,64.6842105263158,
-9.29999999999999));
#26137=CARTESIAN_POINT('Ctrl Pts',(2.49192748960943,64.8815789473684,-9.29999999999999));
#26138=CARTESIAN_POINT('Ctrl Pts',(4.64999999999999,65.078947368421,-8.05403625519527));
#26139=CARTESIAN_POINT('Ctrl Pts',(6.80807251039054,65.2763157894737,-6.80807251039055));
#26140=CARTESIAN_POINT('Ctrl Pts',(8.05403625519526,65.4736842105263,-4.65));
#26141=CARTESIAN_POINT('Ctrl Pts',(9.29999999999998,65.6710526315789,-2.49192748960944));
#26142=CARTESIAN_POINT('Ctrl Pts',(9.29999999999999,65.8684210526316,-1.70838228481055E-15));
#26143=CARTESIAN_POINT('Ctrl Pts',(9.29999999999999,66.0657894736842,2.49192748960943));
#26144=CARTESIAN_POINT('Ctrl Pts',(8.05403625519527,66.2631578947368,4.64999999999998));
#26145=CARTESIAN_POINT('Ctrl Pts',(6.80807251039055,66.4605263157895,6.80807251039054));
#26146=CARTESIAN_POINT('Ctrl Pts',(4.65,66.6578947368421,8.05403625519526));
#26147=CARTESIAN_POINT('Ctrl Pts',(2.49192748960945,66.8552631578947,9.29999999999998));
#26148=CARTESIAN_POINT('Ctrl Pts',(7.90401649176522E-28,67.0526315789473,
9.29999999999999));
#26149=CARTESIAN_POINT('Ctrl Pts',(-2.49192748960944,67.25,9.29999999999998));
#26150=CARTESIAN_POINT('Ctrl Pts',(-4.64999999999999,67.4473684210526,8.05403625519527));
#26151=CARTESIAN_POINT('Ctrl Pts',(-6.80807251039054,67.6447368421052,6.80807251039054));
#26152=CARTESIAN_POINT('Ctrl Pts',(-8.05403625519527,67.8421052631579,4.64999999999999));
#26153=CARTESIAN_POINT('Ctrl Pts',(-9.29999999999998,68.0394736842105,2.49192748960944));
#26154=CARTESIAN_POINT('Ctrl Pts',(-9.29999999999999,68.2368421052632,5.69460761603868E-16));
#26155=CARTESIAN_POINT('Ctrl Pts',(-9.29999999999998,68.4342105263158,-2.49192748960943));
#26156=CARTESIAN_POINT('Ctrl Pts',(-8.05403625519527,68.6315789473684,-4.64999999999999));
#26157=CARTESIAN_POINT('Ctrl Pts',(-6.80807251039054,68.8289473684211,-6.80807251039054));
#26158=CARTESIAN_POINT('Ctrl Pts',(-4.65,69.0263157894737,-8.05403625519526));
#26159=CARTESIAN_POINT('Ctrl Pts',(-2.49192748960944,69.2236842105263,-9.29999999999998));
#26160=CARTESIAN_POINT('Ctrl Pts',(-1.13892152320633E-15,69.421052631579,
-9.29999999999998));
#26161=CARTESIAN_POINT('Ctrl Pts',(2.49192748960943,69.6184210526316,-9.29999999999999));
#26162=CARTESIAN_POINT('Ctrl Pts',(4.64999999999999,69.8157894736842,-8.05403625519526));
#26163=CARTESIAN_POINT('Ctrl Pts',(6.80807251039054,70.0131578947368,-6.80807251039055));
#26164=CARTESIAN_POINT('Ctrl Pts',(8.05403625519526,70.2105263157894,-4.65));
#26165=CARTESIAN_POINT('Ctrl Pts',(9.29999999999998,70.4078947368421,-2.49192748960944));
#26166=CARTESIAN_POINT('Ctrl Pts',(9.29999999999999,70.6052631578947,-1.70838228481055E-15));
#26167=CARTESIAN_POINT('Ctrl Pts',(9.29999999999999,70.8026315789474,2.49192748960943));
#26168=CARTESIAN_POINT('Ctrl Pts',(8.05403625519527,71.,4.64999999999999));
#26169=CARTESIAN_POINT('Ctrl Pts',(6.80807251039055,71.1973684210526,6.80807251039054));
#26170=CARTESIAN_POINT('Ctrl Pts',(4.65,71.3947368421052,8.05403625519526));
#26171=CARTESIAN_POINT('Ctrl Pts',(2.49192748960945,71.5921052631579,9.29999999999998));
#26172=CARTESIAN_POINT('Ctrl Pts',(8.37779525808447E-28,71.7894736842105,
9.29999999999999));
#26173=CARTESIAN_POINT('Ctrl Pts',(-2.49192748960944,71.9868421052631,9.29999999999998));
#26174=CARTESIAN_POINT('Ctrl Pts',(-4.64999999999999,72.1842105263157,8.05403625519527));
#26175=CARTESIAN_POINT('Ctrl Pts',(-6.80807251039054,72.3815789473683,6.80807251039054));
#26176=CARTESIAN_POINT('Ctrl Pts',(-8.05403625519527,72.5789473684211,4.64999999999999));
#26177=CARTESIAN_POINT('Ctrl Pts',(-9.29999999999998,72.7763157894737,2.49192748960944));
#26178=CARTESIAN_POINT('Ctrl Pts',(-9.29999999999999,72.9736842105263,5.6946076160372E-16));
#26179=CARTESIAN_POINT('Ctrl Pts',(-9.29999999999998,73.1710526315789,-2.49192748960943));
#26180=CARTESIAN_POINT('Ctrl Pts',(-8.05403625519527,73.3684210526315,-4.64999999999999));
#26181=CARTESIAN_POINT('Ctrl Pts',(-6.80807251039054,73.5657894736842,-6.80807251039054));
#26182=CARTESIAN_POINT('Ctrl Pts',(-4.65,73.7631578947368,-8.05403625519526));
#26183=CARTESIAN_POINT('Ctrl Pts',(-2.49192748960944,73.9605263157895,-9.29999999999998));
#26184=CARTESIAN_POINT('Ctrl Pts',(-1.13892152320627E-15,74.1578947368421,
-9.29999999999999));
#26185=CARTESIAN_POINT('Ctrl Pts',(2.49192748960943,74.3552631578947,-9.29999999999999));
#26186=CARTESIAN_POINT('Ctrl Pts',(4.64999999999999,74.5526315789473,-8.05403625519527));
#26187=CARTESIAN_POINT('Ctrl Pts',(6.80807251039054,74.75,-6.80807251039055));
#26188=CARTESIAN_POINT('Ctrl Pts',(8.05403625519526,74.9473684210526,-4.65));
#26189=CARTESIAN_POINT('Ctrl Pts',(9.29999999999998,75.1447368421053,-2.49192748960945));
#26190=CARTESIAN_POINT('Ctrl Pts',(9.29999999999999,75.3421052631579,-1.70838228481055E-15));
#26191=CARTESIAN_POINT('Ctrl Pts',(9.29999999999999,75.5394736842105,2.49192748960943));
#26192=CARTESIAN_POINT('Ctrl Pts',(8.05403625519527,75.7368421052631,4.64999999999998));
#26193=CARTESIAN_POINT('Ctrl Pts',(6.80807251039055,75.9342105263157,6.80807251039054));
#26194=CARTESIAN_POINT('Ctrl Pts',(4.65,76.1315789473684,8.05403625519527));
#26195=CARTESIAN_POINT('Ctrl Pts',(2.49192748960945,76.3289473684211,9.29999999999998));
#26196=CARTESIAN_POINT('Ctrl Pts',(8.87468518373638E-28,76.5263157894736,
9.29999999999999));
#26197=CARTESIAN_POINT('Ctrl Pts',(-2.49192748960944,76.7236842105263,9.29999999999998));
#26198=CARTESIAN_POINT('Ctrl Pts',(-4.64999999999999,76.9210526315789,8.05403625519527));
#26199=CARTESIAN_POINT('Ctrl Pts',(-6.80807251039054,77.1184210526315,6.80807251039054));
#26200=CARTESIAN_POINT('Ctrl Pts',(-8.05403625519527,77.3157894736842,4.64999999999999));
#26201=CARTESIAN_POINT('Ctrl Pts',(-9.29999999999998,77.5131578947368,2.49192748960944));
#26202=CARTESIAN_POINT('Ctrl Pts',(-9.29999999999999,77.7105263157894,5.6946076160372E-16));
#26203=CARTESIAN_POINT('Ctrl Pts',(-9.29999999999998,77.9078947368421,-2.49192748960943));
#26204=CARTESIAN_POINT('Ctrl Pts',(-8.05403625519527,78.1052631578947,-4.64999999999999));
#26205=CARTESIAN_POINT('Ctrl Pts',(-6.80807251039054,78.3026315789474,-6.80807251039054));
#26206=CARTESIAN_POINT('Ctrl Pts',(-4.65,78.5,-8.05403625519526));
#26207=CARTESIAN_POINT('Ctrl Pts',(-2.49192748960944,78.6973684210526,-9.29999999999998));
#26208=CARTESIAN_POINT('Ctrl Pts',(-1.13892152320622E-15,78.8947368421053,
-9.29999999999999));
#26209=CARTESIAN_POINT('Ctrl Pts',(2.49192748960943,79.0921052631579,-9.29999999999999));
#26210=CARTESIAN_POINT('Ctrl Pts',(4.64999999999999,79.2894736842105,-8.05403625519527));
#26211=CARTESIAN_POINT('Ctrl Pts',(6.80807251039054,79.4868421052632,-6.80807251039055));
#26212=CARTESIAN_POINT('Ctrl Pts',(8.05403625519526,79.6842105263157,-4.65));
#26213=CARTESIAN_POINT('Ctrl Pts',(9.29999999999998,79.8815789473684,-2.49192748960945));
#26214=CARTESIAN_POINT('Ctrl Pts',(9.29999999999999,80.0789473684211,-1.70838228481055E-15));
#26215=CARTESIAN_POINT('Ctrl Pts',(9.29999999999999,80.2763157894737,2.49192748960943));
#26216=CARTESIAN_POINT('Ctrl Pts',(8.05403625519527,80.4736842105264,4.64999999999998));
#26217=CARTESIAN_POINT('Ctrl Pts',(6.80807251039055,80.6710526315789,6.80807251039054));
#26218=CARTESIAN_POINT('Ctrl Pts',(4.65,80.8684210526316,8.05403625519526));
#26219=CARTESIAN_POINT('Ctrl Pts',(2.49192748960945,81.0657894736842,9.29999999999998));
#26220=CARTESIAN_POINT('Ctrl Pts',(9.36001952972196E-28,81.2631578947368,
9.29999999999999));
#26221=CARTESIAN_POINT('Ctrl Pts',(-2.49192748960944,81.4605263157895,9.29999999999998));
#26222=CARTESIAN_POINT('Ctrl Pts',(-4.64999999999999,81.6578947368421,8.05403625519527));
#26223=CARTESIAN_POINT('Ctrl Pts',(-6.80807251039054,81.8552631578947,6.80807251039054));
#26224=CARTESIAN_POINT('Ctrl Pts',(-8.05403625519527,82.0526315789474,4.64999999999999));
#26225=CARTESIAN_POINT('Ctrl Pts',(-9.29999999999998,82.25,2.49192748960944));
#26226=CARTESIAN_POINT('Ctrl Pts',(-9.29999999999999,82.4473684210526,5.6946076160372E-16));
#26227=CARTESIAN_POINT('Ctrl Pts',(-9.29999999999998,82.6447368421053,-2.49192748960944));
#26228=CARTESIAN_POINT('Ctrl Pts',(-8.05403625519527,82.8421052631579,-4.64999999999999));
#26229=CARTESIAN_POINT('Ctrl Pts',(-6.80807251039054,83.0394736842105,-6.80807251039054));
#26230=CARTESIAN_POINT('Ctrl Pts',(-4.65,83.2368421052631,-8.05403625519526));
#26231=CARTESIAN_POINT('Ctrl Pts',(-2.49192748960944,83.4342105263158,-9.29999999999998));
#26232=CARTESIAN_POINT('Ctrl Pts',(-1.13892152320617E-15,83.6315789473684,
-9.29999999999998));
#26233=CARTESIAN_POINT('Ctrl Pts',(2.49192748960943,83.8289473684211,-9.29999999999999));
#26234=CARTESIAN_POINT('Ctrl Pts',(4.64999999999999,84.0263157894737,-8.05403625519527));
#26235=CARTESIAN_POINT('Ctrl Pts',(6.80807251039054,84.2236842105264,-6.80807251039055));
#26236=CARTESIAN_POINT('Ctrl Pts',(8.05403625519526,84.4210526315789,-4.65));
#26237=CARTESIAN_POINT('Ctrl Pts',(9.29999999999998,84.6184210526316,-2.49192748960945));
#26238=CARTESIAN_POINT('Ctrl Pts',(9.29999999999999,84.8157894736842,-1.7083822848104E-15));
#26239=CARTESIAN_POINT('Ctrl Pts',(9.29999999999999,85.0131578947368,2.49192748960943));
#26240=CARTESIAN_POINT('Ctrl Pts',(8.05403625519527,85.2105263157895,4.64999999999998));
#26241=CARTESIAN_POINT('Ctrl Pts',(6.80807251039055,85.407894736842,6.80807251039054));
#26242=CARTESIAN_POINT('Ctrl Pts',(4.65,85.6052631578947,8.05403625519526));
#26243=CARTESIAN_POINT('Ctrl Pts',(2.49192748960945,85.8026315789473,9.29999999999998));
#26244=CARTESIAN_POINT('Ctrl Pts',(9.98402083170343E-28,86.,9.29999999999999));
#26245=CARTESIAN_POINT('Ctrl Pts',(-1.38666955995881E-29,-3.99999999999997,
5.29999999999999));
#26246=CARTESIAN_POINT('Ctrl Pts',(-1.42013071988495,-3.80263157894733,
5.29999999999999));
#26247=CARTESIAN_POINT('Ctrl Pts',(-2.65,-3.60526315789474,4.58993464005751));
#26248=CARTESIAN_POINT('Ctrl Pts',(-3.87986928011504,-3.40789473684211,
3.87986928011504));
#26249=CARTESIAN_POINT('Ctrl Pts',(-4.58993464005752,-3.21052631578946,
2.65));
#26250=CARTESIAN_POINT('Ctrl Pts',(-5.29999999999999,-3.01315789473685,
1.42013071988495));
#26251=CARTESIAN_POINT('Ctrl Pts',(-5.29999999999999,-2.81578947368422,
3.24531401773979E-16));
#26252=CARTESIAN_POINT('Ctrl Pts',(-5.29999999999999,-2.61842105263159,
-1.42013071988495));
#26253=CARTESIAN_POINT('Ctrl Pts',(-4.58993464005752,-2.42105263157898,
-2.65));
#26254=CARTESIAN_POINT('Ctrl Pts',(-3.87986928011504,-2.22368421052633,
-3.87986928011504));
#26255=CARTESIAN_POINT('Ctrl Pts',(-2.65,-2.02631578947369,-4.58993464005752));
#26256=CARTESIAN_POINT('Ctrl Pts',(-1.42013071988495,-1.82894736842106,
-5.29999999999999));
#26257=CARTESIAN_POINT('Ctrl Pts',(-6.4906280354814E-16,-1.63157894736846,
-5.29999999999999));
#26258=CARTESIAN_POINT('Ctrl Pts',(1.42013071988495,-1.4342105263158,-5.29999999999999));
#26259=CARTESIAN_POINT('Ctrl Pts',(2.65,-1.23684210526317,-4.58993464005752));
#26260=CARTESIAN_POINT('Ctrl Pts',(3.87986928011504,-1.03947368421054,-3.87986928011504));
#26261=CARTESIAN_POINT('Ctrl Pts',(4.58993464005752,-0.842105263157894,
-2.65));
#26262=CARTESIAN_POINT('Ctrl Pts',(5.29999999999999,-0.644736842105277,
-1.42013071988495));
#26263=CARTESIAN_POINT('Ctrl Pts',(5.29999999999999,-0.447368421052613,
-9.73594205322067E-16));
#26264=CARTESIAN_POINT('Ctrl Pts',(5.29999999999999,-0.250000000000015,
1.42013071988495));
#26265=CARTESIAN_POINT('Ctrl Pts',(4.58993464005752,-0.0526315789473736,
2.64999999999999));
#26266=CARTESIAN_POINT('Ctrl Pts',(3.87986928011504,0.14473684210529,3.87986928011504));
#26267=CARTESIAN_POINT('Ctrl Pts',(2.65,0.342105263157907,4.58993464005751));
#26268=CARTESIAN_POINT('Ctrl Pts',(1.42013071988495,0.539473684210552,5.29999999999999));
#26269=CARTESIAN_POINT('Ctrl Pts',(4.16000867987643E-29,0.736842105263188,
5.29999999999999));
#26270=CARTESIAN_POINT('Ctrl Pts',(-1.42013071988495,0.934210526315814,
5.29999999999999));
#26271=CARTESIAN_POINT('Ctrl Pts',(-2.65,1.13157894736843,4.58993464005752));
#26272=CARTESIAN_POINT('Ctrl Pts',(-3.87986928011504,1.32894736842108,3.87986928011504));
#26273=CARTESIAN_POINT('Ctrl Pts',(-4.58993464005752,1.52631578947371,2.65));
#26274=CARTESIAN_POINT('Ctrl Pts',(-5.29999999999999,1.72368421052634,1.42013071988495));
#26275=CARTESIAN_POINT('Ctrl Pts',(-5.29999999999999,1.92105263157895,3.24531401773979E-16));
#26276=CARTESIAN_POINT('Ctrl Pts',(-5.29999999999999,2.11842105263156,-1.42013071988495));
#26277=CARTESIAN_POINT('Ctrl Pts',(-4.58993464005752,2.31578947368419,-2.65));
#26278=CARTESIAN_POINT('Ctrl Pts',(-3.87986928011504,2.51315789473682,-3.87986928011504));
#26279=CARTESIAN_POINT('Ctrl Pts',(-2.65,2.71052631578947,-4.58993464005752));
#26280=CARTESIAN_POINT('Ctrl Pts',(-1.42013071988495,2.90789473684208,-5.29999999999999));
#26281=CARTESIAN_POINT('Ctrl Pts',(-6.49062803548097E-16,3.10526315789471,
-5.3));
#26282=CARTESIAN_POINT('Ctrl Pts',(1.42013071988495,3.30263157894734,-5.29999999999999));
#26283=CARTESIAN_POINT('Ctrl Pts',(2.65,3.49999999999999,-4.58993464005752));
#26284=CARTESIAN_POINT('Ctrl Pts',(3.87986928011504,3.69736842105261,-3.87986928011504));
#26285=CARTESIAN_POINT('Ctrl Pts',(4.58993464005752,3.89473684210527,-2.65));
#26286=CARTESIAN_POINT('Ctrl Pts',(5.29999999999999,4.09210526315787,-1.42013071988495));
#26287=CARTESIAN_POINT('Ctrl Pts',(5.29999999999999,4.28947368421051,-9.73594205322215E-16));
#26288=CARTESIAN_POINT('Ctrl Pts',(5.29999999999999,4.48684210526317,1.42013071988495));
#26289=CARTESIAN_POINT('Ctrl Pts',(4.58993464005752,4.68421052631579,2.64999999999999));
#26290=CARTESIAN_POINT('Ctrl Pts',(3.87986928011504,4.88157894736844,3.87986928011504));
#26291=CARTESIAN_POINT('Ctrl Pts',(2.65,5.07894736842107,4.58993464005752));
#26292=CARTESIAN_POINT('Ctrl Pts',(1.42013071988495,5.2763157894737,5.29999999999999));
#26293=CARTESIAN_POINT('Ctrl Pts',(8.66668474974256E-29,5.47368421052635,
5.29999999999999));
#26294=CARTESIAN_POINT('Ctrl Pts',(-1.42013071988495,5.67105263157896,5.29999999999999));
#26295=CARTESIAN_POINT('Ctrl Pts',(-2.65,5.86842105263159,4.58993464005752));
#26296=CARTESIAN_POINT('Ctrl Pts',(-3.87986928011504,6.06578947368422,3.87986928011504));
#26297=CARTESIAN_POINT('Ctrl Pts',(-4.58993464005752,6.26315789473683,2.65));
#26298=CARTESIAN_POINT('Ctrl Pts',(-5.29999999999999,6.46052631578948,1.42013071988495));
#26299=CARTESIAN_POINT('Ctrl Pts',(-5.29999999999999,6.65789473684211,3.24531401773979E-16));
#26300=CARTESIAN_POINT('Ctrl Pts',(-5.29999999999999,6.85526315789475,-1.42013071988495));
#26301=CARTESIAN_POINT('Ctrl Pts',(-4.58993464005752,7.05263157894735,-2.65));
#26302=CARTESIAN_POINT('Ctrl Pts',(-3.87986928011504,7.24999999999997,-3.87986928011504));
#26303=CARTESIAN_POINT('Ctrl Pts',(-2.65,7.44736842105263,-4.58993464005752));
#26304=CARTESIAN_POINT('Ctrl Pts',(-1.42013071988495,7.64473684210523,-5.29999999999999));
#26305=CARTESIAN_POINT('Ctrl Pts',(-6.49062803548034E-16,7.84210526315787,
-5.29999999999999));
#26306=CARTESIAN_POINT('Ctrl Pts',(1.42013071988495,8.03947368421049,-5.29999999999999));
#26307=CARTESIAN_POINT('Ctrl Pts',(2.65,8.23684210526315,-4.58993464005752));
#26308=CARTESIAN_POINT('Ctrl Pts',(3.87986928011504,8.43421052631579,-3.87986928011504));
#26309=CARTESIAN_POINT('Ctrl Pts',(4.58993464005752,8.63157894736839,-2.65));
#26310=CARTESIAN_POINT('Ctrl Pts',(5.29999999999999,8.82894736842105,-1.42013071988495));
#26311=CARTESIAN_POINT('Ctrl Pts',(5.29999999999999,9.02631578947367,-9.73594205322215E-16));
#26312=CARTESIAN_POINT('Ctrl Pts',(5.29999999999999,9.22368421052632,1.42013071988494));
#26313=CARTESIAN_POINT('Ctrl Pts',(4.58993464005752,9.42105263157895,2.64999999999999));
#26314=CARTESIAN_POINT('Ctrl Pts',(3.87986928011504,9.61842105263158,3.87986928011504));
#26315=CARTESIAN_POINT('Ctrl Pts',(2.65,9.81578947368424,4.58993464005751));
#26316=CARTESIAN_POINT('Ctrl Pts',(1.42013071988495,10.0131578947368,5.29999999999999));
#26317=CARTESIAN_POINT('Ctrl Pts',(1.45600303795675E-28,10.2105263157895,
5.29999999999999));
#26318=CARTESIAN_POINT('Ctrl Pts',(-1.42013071988495,10.4078947368421,5.29999999999999));
#26319=CARTESIAN_POINT('Ctrl Pts',(-2.65,10.6052631578948,4.58993464005751));
#26320=CARTESIAN_POINT('Ctrl Pts',(-3.87986928011504,10.8026315789474,3.87986928011504));
#26321=CARTESIAN_POINT('Ctrl Pts',(-4.58993464005752,11.,2.65));
#26322=CARTESIAN_POINT('Ctrl Pts',(-5.29999999999999,11.1973684210526,1.42013071988495));
#26323=CARTESIAN_POINT('Ctrl Pts',(-5.29999999999999,11.3947368421053,3.24531401773979E-16));
#26324=CARTESIAN_POINT('Ctrl Pts',(-5.29999999999999,11.5921052631579,-1.42013071988495));
#26325=CARTESIAN_POINT('Ctrl Pts',(-4.58993464005752,11.7894736842105,-2.64999999999999));
#26326=CARTESIAN_POINT('Ctrl Pts',(-3.87986928011504,11.9868421052632,-3.87986928011504));
#26327=CARTESIAN_POINT('Ctrl Pts',(-2.65,12.1842105263158,-4.58993464005752));
#26328=CARTESIAN_POINT('Ctrl Pts',(-1.42013071988495,12.3815789473684,-5.29999999999999));
#26329=CARTESIAN_POINT('Ctrl Pts',(-6.4906280354798E-16,12.578947368421,
-5.3));
#26330=CARTESIAN_POINT('Ctrl Pts',(1.42013071988495,12.7763157894737,-5.29999999999999));
#26331=CARTESIAN_POINT('Ctrl Pts',(2.65,12.9736842105263,-4.58993464005752));
#26332=CARTESIAN_POINT('Ctrl Pts',(3.87986928011504,13.1710526315789,-3.87986928011504));
#26333=CARTESIAN_POINT('Ctrl Pts',(4.58993464005752,13.3684210526316,-2.65));
#26334=CARTESIAN_POINT('Ctrl Pts',(5.29999999999999,13.5657894736842,-1.42013071988495));
#26335=CARTESIAN_POINT('Ctrl Pts',(5.29999999999999,13.7631578947368,-9.73594205322067E-16));
#26336=CARTESIAN_POINT('Ctrl Pts',(5.29999999999999,13.9605263157895,1.42013071988495));
#26337=CARTESIAN_POINT('Ctrl Pts',(4.58993464005752,14.1578947368421,2.64999999999999));
#26338=CARTESIAN_POINT('Ctrl Pts',(3.87986928011504,14.3552631578948,3.87986928011504));
#26339=CARTESIAN_POINT('Ctrl Pts',(2.65,14.5526315789474,4.58993464005752));
#26340=CARTESIAN_POINT('Ctrl Pts',(1.42013071988495,14.75,5.3));
#26341=CARTESIAN_POINT('Ctrl Pts',(1.94133738394233E-28,14.9473684210526,
5.29999999999999));
#26342=CARTESIAN_POINT('Ctrl Pts',(-1.42013071988495,15.1447368421053,5.3));
#26343=CARTESIAN_POINT('Ctrl Pts',(-2.65,15.3421052631579,4.58993464005752));
#26344=CARTESIAN_POINT('Ctrl Pts',(-3.87986928011504,15.5394736842106,3.87986928011505));
#26345=CARTESIAN_POINT('Ctrl Pts',(-4.58993464005752,15.7368421052632,2.65));
#26346=CARTESIAN_POINT('Ctrl Pts',(-5.29999999999999,15.9342105263158,1.42013071988495));
#26347=CARTESIAN_POINT('Ctrl Pts',(-5.29999999999999,16.1315789473684,3.24531401773979E-16));
#26348=CARTESIAN_POINT('Ctrl Pts',(-5.29999999999999,16.328947368421,-1.42013071988495));
#26349=CARTESIAN_POINT('Ctrl Pts',(-4.58993464005752,16.5263157894737,-2.64999999999999));
#26350=CARTESIAN_POINT('Ctrl Pts',(-3.87986928011504,16.7236842105263,-3.87986928011504));
#26351=CARTESIAN_POINT('Ctrl Pts',(-2.65,16.9210526315789,-4.58993464005752));
#26352=CARTESIAN_POINT('Ctrl Pts',(-1.42013071988495,17.1184210526316,-5.29999999999999));
#26353=CARTESIAN_POINT('Ctrl Pts',(-6.49062803547937E-16,17.3157894736842,
-5.3));
#26354=CARTESIAN_POINT('Ctrl Pts',(1.42013071988495,17.5131578947368,-5.29999999999999));
#26355=CARTESIAN_POINT('Ctrl Pts',(2.65,17.7105263157894,-4.58993464005752));
#26356=CARTESIAN_POINT('Ctrl Pts',(3.87986928011504,17.9078947368421,-3.87986928011504));
#26357=CARTESIAN_POINT('Ctrl Pts',(4.58993464005752,18.1052631578947,-2.65));
#26358=CARTESIAN_POINT('Ctrl Pts',(5.29999999999999,18.3026315789473,-1.42013071988495));
#26359=CARTESIAN_POINT('Ctrl Pts',(5.29999999999999,18.5,-9.73594205322067E-16));
#26360=CARTESIAN_POINT('Ctrl Pts',(5.29999999999999,18.6973684210526,1.42013071988495));
#26361=CARTESIAN_POINT('Ctrl Pts',(4.58993464005752,18.8947368421053,2.64999999999999));
#26362=CARTESIAN_POINT('Ctrl Pts',(3.87986928011504,19.0921052631579,3.87986928011504));
#26363=CARTESIAN_POINT('Ctrl Pts',(2.65,19.2894736842105,4.58993464005751));
#26364=CARTESIAN_POINT('Ctrl Pts',(1.42013071988495,19.4868421052632,5.29999999999999));
#26365=CARTESIAN_POINT('Ctrl Pts',(2.42667172992792E-28,19.6842105263158,
5.29999999999999));
#26366=CARTESIAN_POINT('Ctrl Pts',(-1.42013071988495,19.8815789473684,5.29999999999999));
#26367=CARTESIAN_POINT('Ctrl Pts',(-2.65,20.0789473684211,4.58993464005751));
#26368=CARTESIAN_POINT('Ctrl Pts',(-3.87986928011504,20.2763157894737,3.87986928011504));
#26369=CARTESIAN_POINT('Ctrl Pts',(-4.58993464005752,20.4736842105263,2.65));
#26370=CARTESIAN_POINT('Ctrl Pts',(-5.29999999999999,20.671052631579,1.42013071988495));
#26371=CARTESIAN_POINT('Ctrl Pts',(-5.29999999999999,20.8684210526316,3.24531401773979E-16));
#26372=CARTESIAN_POINT('Ctrl Pts',(-5.29999999999999,21.0657894736842,-1.42013071988495));
#26373=CARTESIAN_POINT('Ctrl Pts',(-4.58993464005752,21.2631578947368,-2.65));
#26374=CARTESIAN_POINT('Ctrl Pts',(-3.87986928011504,21.4605263157894,-3.87986928011504));
#26375=CARTESIAN_POINT('Ctrl Pts',(-2.65,21.6578947368421,-4.58993464005752));
#26376=CARTESIAN_POINT('Ctrl Pts',(-1.42013071988495,21.8552631578947,-5.29999999999999));
#26377=CARTESIAN_POINT('Ctrl Pts',(-6.49062803547882E-16,22.0526315789474,
-5.29999999999999));
#26378=CARTESIAN_POINT('Ctrl Pts',(1.42013071988495,22.25,-5.29999999999999));
#26379=CARTESIAN_POINT('Ctrl Pts',(2.65,22.4473684210526,-4.58993464005752));
#26380=CARTESIAN_POINT('Ctrl Pts',(3.87986928011504,22.6447368421052,-3.87986928011504));
#26381=CARTESIAN_POINT('Ctrl Pts',(4.58993464005752,22.8421052631579,-2.65));
#26382=CARTESIAN_POINT('Ctrl Pts',(5.29999999999999,23.0394736842105,-1.42013071988495));
#26383=CARTESIAN_POINT('Ctrl Pts',(5.29999999999999,23.2368421052632,-9.73594205322067E-16));
#26384=CARTESIAN_POINT('Ctrl Pts',(5.29999999999999,23.4342105263158,1.42013071988495));
#26385=CARTESIAN_POINT('Ctrl Pts',(4.58993464005752,23.6315789473684,2.64999999999999));
#26386=CARTESIAN_POINT('Ctrl Pts',(3.87986928011504,23.8289473684211,3.87986928011504));
#26387=CARTESIAN_POINT('Ctrl Pts',(2.65,24.0263157894737,4.58993464005752));
#26388=CARTESIAN_POINT('Ctrl Pts',(1.42013071988495,24.2236842105263,5.29999999999999));
#26389=CARTESIAN_POINT('Ctrl Pts',(2.9120060759135E-28,24.421052631579,
5.29999999999999));
#26390=CARTESIAN_POINT('Ctrl Pts',(-1.42013071988495,24.6184210526316,5.29999999999999));
#26391=CARTESIAN_POINT('Ctrl Pts',(-2.65,24.8157894736842,4.58993464005752));
#26392=CARTESIAN_POINT('Ctrl Pts',(-3.87986928011504,25.0131578947368,3.87986928011504));
#26393=CARTESIAN_POINT('Ctrl Pts',(-4.58993464005752,25.2105263157895,2.65));
#26394=CARTESIAN_POINT('Ctrl Pts',(-5.29999999999999,25.4078947368421,1.42013071988495));
#26395=CARTESIAN_POINT('Ctrl Pts',(-5.29999999999999,25.6052631578947,3.24531401773979E-16));
#26396=CARTESIAN_POINT('Ctrl Pts',(-5.29999999999999,25.8026315789474,-1.42013071988495));
#26397=CARTESIAN_POINT('Ctrl Pts',(-4.58993464005752,26.,-2.65));
#26398=CARTESIAN_POINT('Ctrl Pts',(-3.87986928011504,26.1973684210526,-3.87986928011504));
#26399=CARTESIAN_POINT('Ctrl Pts',(-2.65,26.3947368421052,-4.58993464005752));
#26400=CARTESIAN_POINT('Ctrl Pts',(-1.42013071988495,26.5921052631579,-5.29999999999999));
#26401=CARTESIAN_POINT('Ctrl Pts',(-6.49062803547835E-16,26.7894736842105,
-5.3));
#26402=CARTESIAN_POINT('Ctrl Pts',(1.42013071988495,26.9868421052632,-5.29999999999999));
#26403=CARTESIAN_POINT('Ctrl Pts',(2.65,27.1842105263158,-4.58993464005752));
#26404=CARTESIAN_POINT('Ctrl Pts',(3.87986928011504,27.3815789473684,-3.87986928011504));
#26405=CARTESIAN_POINT('Ctrl Pts',(4.58993464005752,27.578947368421,-2.65));
#26406=CARTESIAN_POINT('Ctrl Pts',(5.29999999999999,27.7763157894737,-1.42013071988495));
#26407=CARTESIAN_POINT('Ctrl Pts',(5.29999999999999,27.9736842105263,-9.73594205322067E-16));
#26408=CARTESIAN_POINT('Ctrl Pts',(5.29999999999999,28.1710526315789,1.42013071988494));
#26409=CARTESIAN_POINT('Ctrl Pts',(4.58993464005752,28.3684210526316,2.64999999999999));
#26410=CARTESIAN_POINT('Ctrl Pts',(3.87986928011504,28.5657894736842,3.87986928011504));
#26411=CARTESIAN_POINT('Ctrl Pts',(2.65,28.7631578947368,4.58993464005752));
#26412=CARTESIAN_POINT('Ctrl Pts',(1.42013071988495,28.9605263157895,5.29999999999999));
#26413=CARTESIAN_POINT('Ctrl Pts',(3.48978505922967E-28,29.1578947368422,
5.29999999999999));
#26414=CARTESIAN_POINT('Ctrl Pts',(-1.42013071988495,29.3552631578947,5.29999999999999));
#26415=CARTESIAN_POINT('Ctrl Pts',(-2.65,29.5526315789474,4.58993464005751));
#26416=CARTESIAN_POINT('Ctrl Pts',(-3.87986928011504,29.75,3.87986928011504));
#26417=CARTESIAN_POINT('Ctrl Pts',(-4.58993464005752,29.9473684210527,2.65));
#26418=CARTESIAN_POINT('Ctrl Pts',(-5.29999999999999,30.1447368421053,1.42013071988495));
#26419=CARTESIAN_POINT('Ctrl Pts',(-5.29999999999999,30.3421052631579,3.24531401773979E-16));
#26420=CARTESIAN_POINT('Ctrl Pts',(-5.29999999999999,30.5394736842105,-1.42013071988495));
#26421=CARTESIAN_POINT('Ctrl Pts',(-4.58993464005752,30.7368421052631,-2.65));
#26422=CARTESIAN_POINT('Ctrl Pts',(-3.87986928011504,30.9342105263158,-3.87986928011504));
#26423=CARTESIAN_POINT('Ctrl Pts',(-2.65,31.1315789473684,-4.58993464005752));
#26424=CARTESIAN_POINT('Ctrl Pts',(-1.42013071988495,31.328947368421,-5.29999999999999));
#26425=CARTESIAN_POINT('Ctrl Pts',(-6.49062803547778E-16,31.5263157894736,
-5.29999999999999));
#26426=CARTESIAN_POINT('Ctrl Pts',(1.42013071988495,31.7236842105263,-5.29999999999999));
#26427=CARTESIAN_POINT('Ctrl Pts',(2.65,31.9210526315789,-4.58993464005752));
#26428=CARTESIAN_POINT('Ctrl Pts',(3.87986928011504,32.1184210526316,-3.87986928011504));
#26429=CARTESIAN_POINT('Ctrl Pts',(4.58993464005752,32.3157894736842,-2.65));
#26430=CARTESIAN_POINT('Ctrl Pts',(5.29999999999999,32.5131578947368,-1.42013071988495));
#26431=CARTESIAN_POINT('Ctrl Pts',(5.29999999999999,32.7105263157895,-9.73594205322215E-16));
#26432=CARTESIAN_POINT('Ctrl Pts',(5.29999999999999,32.9078947368421,1.42013071988495));
#26433=CARTESIAN_POINT('Ctrl Pts',(4.58993464005752,33.1052631578947,2.64999999999999));
#26434=CARTESIAN_POINT('Ctrl Pts',(3.87986928011504,33.3026315789474,3.87986928011504));
#26435=CARTESIAN_POINT('Ctrl Pts',(2.65,33.5,4.58993464005751));
#26436=CARTESIAN_POINT('Ctrl Pts',(1.42013071988495,33.6973684210527,5.29999999999999));
#26437=CARTESIAN_POINT('Ctrl Pts',(4.06756404254584E-28,33.8947368421053,
5.29999999999999));
#26438=CARTESIAN_POINT('Ctrl Pts',(-1.42013071988495,34.0921052631579,5.29999999999999));
#26439=CARTESIAN_POINT('Ctrl Pts',(-2.65,34.2894736842105,4.58993464005752));
#26440=CARTESIAN_POINT('Ctrl Pts',(-3.87986928011504,34.4868421052632,3.87986928011504));
#26441=CARTESIAN_POINT('Ctrl Pts',(-4.58993464005752,34.6842105263158,2.65));
#26442=CARTESIAN_POINT('Ctrl Pts',(-5.29999999999999,34.8815789473684,1.42013071988495));
#26443=CARTESIAN_POINT('Ctrl Pts',(-5.29999999999999,35.078947368421,3.24531401773979E-16));
#26444=CARTESIAN_POINT('Ctrl Pts',(-5.29999999999999,35.2763157894737,-1.42013071988495));
#26445=CARTESIAN_POINT('Ctrl Pts',(-4.58993464005752,35.4736842105263,-2.65));
#26446=CARTESIAN_POINT('Ctrl Pts',(-3.87986928011504,35.6710526315789,-3.87986928011504));
#26447=CARTESIAN_POINT('Ctrl Pts',(-2.65,35.8684210526316,-4.58993464005752));
#26448=CARTESIAN_POINT('Ctrl Pts',(-1.42013071988495,36.0657894736842,-5.29999999999999));
#26449=CARTESIAN_POINT('Ctrl Pts',(-6.4906280354773E-16,36.2631578947368,
-5.3));
#26450=CARTESIAN_POINT('Ctrl Pts',(1.42013071988495,36.4605263157895,-5.29999999999999));
#26451=CARTESIAN_POINT('Ctrl Pts',(2.65,36.6578947368421,-4.58993464005752));
#26452=CARTESIAN_POINT('Ctrl Pts',(3.87986928011504,36.8552631578947,-3.87986928011504));
#26453=CARTESIAN_POINT('Ctrl Pts',(4.58993464005752,37.0526315789474,-2.65));
#26454=CARTESIAN_POINT('Ctrl Pts',(5.29999999999999,37.25,-1.42013071988495));
#26455=CARTESIAN_POINT('Ctrl Pts',(5.29999999999999,37.4473684210526,-9.73594205322067E-16));
#26456=CARTESIAN_POINT('Ctrl Pts',(5.29999999999999,37.6447368421053,1.42013071988495));
#26457=CARTESIAN_POINT('Ctrl Pts',(4.58993464005752,37.8421052631579,2.64999999999999));
#26458=CARTESIAN_POINT('Ctrl Pts',(3.87986928011504,38.0394736842105,3.87986928011504));
#26459=CARTESIAN_POINT('Ctrl Pts',(2.65,38.2368421052632,4.58993464005752));
#26460=CARTESIAN_POINT('Ctrl Pts',(1.42013071988495,38.4342105263158,5.29999999999999));
#26461=CARTESIAN_POINT('Ctrl Pts',(4.50667606986613E-28,38.6315789473685,
5.29999999999999));
#26462=CARTESIAN_POINT('Ctrl Pts',(-1.42013071988495,38.8289473684211,5.29999999999999));
#26463=CARTESIAN_POINT('Ctrl Pts',(-2.65,39.0263157894737,4.58993464005752));
#26464=CARTESIAN_POINT('Ctrl Pts',(-3.87986928011504,39.2236842105263,3.87986928011504));
#26465=CARTESIAN_POINT('Ctrl Pts',(-4.58993464005752,39.4210526315789,2.65));
#26466=CARTESIAN_POINT('Ctrl Pts',(-5.29999999999999,39.6184210526316,1.42013071988495));
#26467=CARTESIAN_POINT('Ctrl Pts',(-5.29999999999999,39.8157894736842,3.24531401773979E-16));
#26468=CARTESIAN_POINT('Ctrl Pts',(-5.29999999999999,40.0131578947369,-1.42013071988495));
#26469=CARTESIAN_POINT('Ctrl Pts',(-4.58993464005752,40.2105263157895,-2.64999999999999));
#26470=CARTESIAN_POINT('Ctrl Pts',(-3.87986928011504,40.4078947368421,-3.87986928011504));
#26471=CARTESIAN_POINT('Ctrl Pts',(-2.65,40.6052631578947,-4.58993464005752));
#26472=CARTESIAN_POINT('Ctrl Pts',(-1.42013071988495,40.8026315789473,-5.29999999999999));
#26473=CARTESIAN_POINT('Ctrl Pts',(-6.49062803547674E-16,40.9999999999999,
-5.29999999999999));
#26474=CARTESIAN_POINT('Ctrl Pts',(1.42013071988495,41.1973684210526,-5.29999999999999));
#26475=CARTESIAN_POINT('Ctrl Pts',(2.65,41.3947368421053,-4.58993464005752));
#26476=CARTESIAN_POINT('Ctrl Pts',(3.87986928011504,41.5921052631579,-3.87986928011504));
#26477=CARTESIAN_POINT('Ctrl Pts',(4.58993464005752,41.7894736842105,-2.65));
#26478=CARTESIAN_POINT('Ctrl Pts',(5.29999999999999,41.9868421052632,-1.42013071988495));
#26479=CARTESIAN_POINT('Ctrl Pts',(5.29999999999999,42.1842105263158,-9.73594205322067E-16));
#26480=CARTESIAN_POINT('Ctrl Pts',(5.29999999999999,42.3815789473684,1.42013071988495));
#26481=CARTESIAN_POINT('Ctrl Pts',(4.58993464005752,42.5789473684211,2.64999999999999));
#26482=CARTESIAN_POINT('Ctrl Pts',(3.87986928011504,42.7763157894737,3.87986928011504));
#26483=CARTESIAN_POINT('Ctrl Pts',(2.65,42.9736842105263,4.58993464005751));
#26484=CARTESIAN_POINT('Ctrl Pts',(1.42013071988495,43.1710526315789,5.29999999999999));
#26485=CARTESIAN_POINT('Ctrl Pts',(5.06134389384965E-28,43.3684210526316,
5.29999999999999));
#26486=CARTESIAN_POINT('Ctrl Pts',(-1.42013071988495,43.5657894736842,5.29999999999999));
#26487=CARTESIAN_POINT('Ctrl Pts',(-2.65,43.7631578947369,4.58993464005751));
#26488=CARTESIAN_POINT('Ctrl Pts',(-3.87986928011504,43.9605263157895,3.87986928011504));
#26489=CARTESIAN_POINT('Ctrl Pts',(-4.58993464005752,44.1578947368421,2.65));
#26490=CARTESIAN_POINT('Ctrl Pts',(-5.29999999999999,44.3552631578947,1.42013071988495));
#26491=CARTESIAN_POINT('Ctrl Pts',(-5.29999999999999,44.5526315789474,3.24531401774127E-16));
#26492=CARTESIAN_POINT('Ctrl Pts',(-5.29999999999999,44.75,-1.42013071988495));
#26493=CARTESIAN_POINT('Ctrl Pts',(-4.58993464005752,44.9473684210526,-2.64999999999999));
#26494=CARTESIAN_POINT('Ctrl Pts',(-3.87986928011504,45.1447368421053,-3.87986928011504));
#26495=CARTESIAN_POINT('Ctrl Pts',(-2.65,45.3421052631579,-4.58993464005752));
#26496=CARTESIAN_POINT('Ctrl Pts',(-1.42013071988495,45.5394736842105,-5.29999999999999));
#26497=CARTESIAN_POINT('Ctrl Pts',(-6.4906280354762E-16,45.7368421052632,
-5.29999999999999));
#26498=CARTESIAN_POINT('Ctrl Pts',(1.42013071988495,45.9342105263158,-5.29999999999999));
#26499=CARTESIAN_POINT('Ctrl Pts',(2.65,46.1315789473684,-4.58993464005752));
#26500=CARTESIAN_POINT('Ctrl Pts',(3.87986928011504,46.328947368421,-3.87986928011504));
#26501=CARTESIAN_POINT('Ctrl Pts',(4.58993464005752,46.5263157894737,-2.65));
#26502=CARTESIAN_POINT('Ctrl Pts',(5.29999999999999,46.7236842105263,-1.42013071988495));
#26503=CARTESIAN_POINT('Ctrl Pts',(5.29999999999999,46.9210526315789,-9.73594205322067E-16));
#26504=CARTESIAN_POINT('Ctrl Pts',(5.29999999999999,47.1184210526316,1.42013071988494));
#26505=CARTESIAN_POINT('Ctrl Pts',(4.58993464005752,47.3157894736842,2.64999999999999));
#26506=CARTESIAN_POINT('Ctrl Pts',(3.87986928011504,47.5131578947369,3.87986928011504));
#26507=CARTESIAN_POINT('Ctrl Pts',(2.65,47.7105263157895,4.58993464005752));
#26508=CARTESIAN_POINT('Ctrl Pts',(1.42013071988495,47.9078947368421,5.29999999999999));
#26509=CARTESIAN_POINT('Ctrl Pts',(5.54667823983524E-28,48.1052631578947,
5.29999999999999));
#26510=CARTESIAN_POINT('Ctrl Pts',(-1.42013071988495,48.3026315789474,5.29999999999999));
#26511=CARTESIAN_POINT('Ctrl Pts',(-2.65,48.5,4.58993464005752));
#26512=CARTESIAN_POINT('Ctrl Pts',(-3.87986928011504,48.6973684210527,3.87986928011505));
#26513=CARTESIAN_POINT('Ctrl Pts',(-4.58993464005752,48.8947368421053,2.65));
#26514=CARTESIAN_POINT('Ctrl Pts',(-5.29999999999999,49.0921052631579,1.42013071988495));
#26515=CARTESIAN_POINT('Ctrl Pts',(-5.29999999999999,49.2894736842105,3.24531401773979E-16));
#26516=CARTESIAN_POINT('Ctrl Pts',(-5.29999999999999,49.4868421052632,-1.42013071988495));
#26517=CARTESIAN_POINT('Ctrl Pts',(-4.58993464005752,49.6842105263158,-2.65));
#26518=CARTESIAN_POINT('Ctrl Pts',(-3.87986928011504,49.8815789473684,-3.87986928011504));
#26519=CARTESIAN_POINT('Ctrl Pts',(-2.65,50.078947368421,-4.58993464005752));
#26520=CARTESIAN_POINT('Ctrl Pts',(-1.42013071988495,50.2763157894736,-5.29999999999999));
#26521=CARTESIAN_POINT('Ctrl Pts',(-6.49062803547577E-16,50.4736842105263,
-5.3));
#26522=CARTESIAN_POINT('Ctrl Pts',(1.42013071988495,50.6710526315789,-5.29999999999999));
#26523=CARTESIAN_POINT('Ctrl Pts',(2.65,50.8684210526316,-4.58993464005752));
#26524=CARTESIAN_POINT('Ctrl Pts',(3.87986928011504,51.0657894736842,-3.87986928011504));
#26525=CARTESIAN_POINT('Ctrl Pts',(4.58993464005752,51.2631578947368,-2.65));
#26526=CARTESIAN_POINT('Ctrl Pts',(5.29999999999999,51.4605263157895,-1.42013071988495));
#26527=CARTESIAN_POINT('Ctrl Pts',(5.29999999999999,51.6578947368421,-9.73594205321919E-16));
#26528=CARTESIAN_POINT('Ctrl Pts',(5.29999999999999,51.8552631578948,1.42013071988495));
#26529=CARTESIAN_POINT('Ctrl Pts',(4.58993464005752,52.0526315789474,2.64999999999999));
#26530=CARTESIAN_POINT('Ctrl Pts',(3.87986928011504,52.25,3.87986928011504));
#26531=CARTESIAN_POINT('Ctrl Pts',(2.65,52.4473684210527,4.58993464005751));
#26532=CARTESIAN_POINT('Ctrl Pts',(1.42013071988495,52.6447368421053,5.29999999999999));
#26533=CARTESIAN_POINT('Ctrl Pts',(6.07823490448612E-28,52.842105263158,
5.29999999999999));
#26534=CARTESIAN_POINT('Ctrl Pts',(-1.42013071988495,53.0394736842106,5.29999999999999));
#26535=CARTESIAN_POINT('Ctrl Pts',(-2.65,53.2368421052632,4.58993464005751));
#26536=CARTESIAN_POINT('Ctrl Pts',(-3.87986928011504,53.4342105263158,3.87986928011504));
#26537=CARTESIAN_POINT('Ctrl Pts',(-4.58993464005752,53.6315789473684,2.65));
#26538=CARTESIAN_POINT('Ctrl Pts',(-5.29999999999999,53.8289473684211,1.42013071988495));
#26539=CARTESIAN_POINT('Ctrl Pts',(-5.29999999999999,54.0263157894737,3.24531401773979E-16));
#26540=CARTESIAN_POINT('Ctrl Pts',(-5.29999999999999,54.2236842105263,-1.42013071988495));
#26541=CARTESIAN_POINT('Ctrl Pts',(-4.58993464005752,54.4210526315789,-2.65));
#26542=CARTESIAN_POINT('Ctrl Pts',(-3.87986928011504,54.6184210526315,-3.87986928011504));
#26543=CARTESIAN_POINT('Ctrl Pts',(-2.65,54.8157894736842,-4.58993464005752));
#26544=CARTESIAN_POINT('Ctrl Pts',(-1.42013071988495,55.0131578947368,-5.29999999999999));
#26545=CARTESIAN_POINT('Ctrl Pts',(-6.49062803547515E-16,55.2105263157894,
-5.29999999999999));
#26546=CARTESIAN_POINT('Ctrl Pts',(1.42013071988495,55.4078947368421,-5.29999999999999));
#26547=CARTESIAN_POINT('Ctrl Pts',(2.65,55.6052631578947,-4.58993464005752));
#26548=CARTESIAN_POINT('Ctrl Pts',(3.87986928011504,55.8026315789474,-3.87986928011504));
#26549=CARTESIAN_POINT('Ctrl Pts',(4.58993464005752,56.,-2.65));
#26550=CARTESIAN_POINT('Ctrl Pts',(5.29999999999999,56.1973684210526,-1.42013071988495));
#26551=CARTESIAN_POINT('Ctrl Pts',(5.29999999999999,56.3947368421052,-9.73594205322067E-16));
#26552=CARTESIAN_POINT('Ctrl Pts',(5.29999999999999,56.5921052631579,1.42013071988495));
#26553=CARTESIAN_POINT('Ctrl Pts',(4.58993464005752,56.7894736842105,2.64999999999999));
#26554=CARTESIAN_POINT('Ctrl Pts',(3.87986928011504,56.9868421052632,3.87986928011504));
#26555=CARTESIAN_POINT('Ctrl Pts',(2.65,57.1842105263158,4.58993464005751));
#26556=CARTESIAN_POINT('Ctrl Pts',(1.42013071988495,57.3815789473684,5.29999999999999));
#26557=CARTESIAN_POINT('Ctrl Pts',(6.58668040980435E-28,57.5789473684211,
5.29999999999999));
#26558=CARTESIAN_POINT('Ctrl Pts',(-1.42013071988495,57.7763157894737,5.29999999999999));
#26559=CARTESIAN_POINT('Ctrl Pts',(-2.65,57.9736842105264,4.58993464005752));
#26560=CARTESIAN_POINT('Ctrl Pts',(-3.87986928011504,58.171052631579,3.87986928011505));
#26561=CARTESIAN_POINT('Ctrl Pts',(-4.58993464005752,58.3684210526316,2.65));
#26562=CARTESIAN_POINT('Ctrl Pts',(-5.29999999999999,58.5657894736842,1.42013071988495));
#26563=CARTESIAN_POINT('Ctrl Pts',(-5.29999999999999,58.7631578947368,3.24531401774127E-16));
#26564=CARTESIAN_POINT('Ctrl Pts',(-5.29999999999999,58.9605263157895,-1.42013071988495));
#26565=CARTESIAN_POINT('Ctrl Pts',(-4.58993464005752,59.1578947368421,-2.65));
#26566=CARTESIAN_POINT('Ctrl Pts',(-3.87986928011504,59.3552631578947,-3.87986928011504));
#26567=CARTESIAN_POINT('Ctrl Pts',(-2.65,59.5526315789473,-4.58993464005752));
#26568=CARTESIAN_POINT('Ctrl Pts',(-1.42013071988495,59.7499999999999,-5.29999999999999));
#26569=CARTESIAN_POINT('Ctrl Pts',(-6.49062803547467E-16,59.9473684210526,
-5.3));
#26570=CARTESIAN_POINT('Ctrl Pts',(1.42013071988495,60.1447368421052,-5.29999999999999));
#26571=CARTESIAN_POINT('Ctrl Pts',(2.65,60.3421052631579,-4.58993464005752));
#26572=CARTESIAN_POINT('Ctrl Pts',(3.87986928011504,60.5394736842105,-3.87986928011504));
#26573=CARTESIAN_POINT('Ctrl Pts',(4.58993464005752,60.7368421052632,-2.65));
#26574=CARTESIAN_POINT('Ctrl Pts',(5.29999999999999,60.9342105263158,-1.42013071988495));
#26575=CARTESIAN_POINT('Ctrl Pts',(5.29999999999999,61.1315789473684,-9.73594205321919E-16));
#26576=CARTESIAN_POINT('Ctrl Pts',(5.29999999999999,61.328947368421,1.42013071988495));
#26577=CARTESIAN_POINT('Ctrl Pts',(4.58993464005752,61.5263157894737,2.64999999999999));
#26578=CARTESIAN_POINT('Ctrl Pts',(3.87986928011504,61.7236842105263,3.87986928011504));
#26579=CARTESIAN_POINT('Ctrl Pts',(2.65,61.921052631579,4.58993464005752));
#26580=CARTESIAN_POINT('Ctrl Pts',(1.42013071988495,62.1184210526316,5.29999999999999));
#26581=CARTESIAN_POINT('Ctrl Pts',(7.14134823378787E-28,62.3157894736843,
5.29999999999999));
#26582=CARTESIAN_POINT('Ctrl Pts',(-1.42013071988495,62.5131578947369,5.29999999999999));
#26583=CARTESIAN_POINT('Ctrl Pts',(-2.65,62.7105263157895,4.58993464005751));
#26584=CARTESIAN_POINT('Ctrl Pts',(-3.87986928011504,62.9078947368421,3.87986928011504));
#26585=CARTESIAN_POINT('Ctrl Pts',(-4.58993464005752,63.1052631578947,2.65));
#26586=CARTESIAN_POINT('Ctrl Pts',(-5.29999999999999,63.3026315789474,1.42013071988495));
#26587=CARTESIAN_POINT('Ctrl Pts',(-5.29999999999999,63.5,3.24531401774127E-16));
#26588=CARTESIAN_POINT('Ctrl Pts',(-5.29999999999999,63.6973684210526,-1.42013071988495));
#26589=CARTESIAN_POINT('Ctrl Pts',(-4.58993464005752,63.8947368421052,-2.65));
#26590=CARTESIAN_POINT('Ctrl Pts',(-3.87986928011504,64.0921052631579,-3.87986928011504));
#26591=CARTESIAN_POINT('Ctrl Pts',(-2.65,64.2894736842104,-4.58993464005752));
#26592=CARTESIAN_POINT('Ctrl Pts',(-1.42013071988495,64.4868421052631,-5.29999999999999));
#26593=CARTESIAN_POINT('Ctrl Pts',(-6.49062803547417E-16,64.6842105263157,
-5.29999999999999));
#26594=CARTESIAN_POINT('Ctrl Pts',(1.42013071988495,64.8815789473684,-5.29999999999999));
#26595=CARTESIAN_POINT('Ctrl Pts',(2.65,65.078947368421,-4.58993464005752));
#26596=CARTESIAN_POINT('Ctrl Pts',(3.87986928011504,65.2763157894737,-3.87986928011504));
#26597=CARTESIAN_POINT('Ctrl Pts',(4.58993464005752,65.4736842105263,-2.65));
#26598=CARTESIAN_POINT('Ctrl Pts',(5.29999999999999,65.6710526315789,-1.42013071988495));
#26599=CARTESIAN_POINT('Ctrl Pts',(5.29999999999999,65.8684210526316,-9.73594205322067E-16));
#26600=CARTESIAN_POINT('Ctrl Pts',(5.29999999999999,66.0657894736842,1.42013071988495));
#26601=CARTESIAN_POINT('Ctrl Pts',(4.58993464005752,66.2631578947368,2.64999999999999));
#26602=CARTESIAN_POINT('Ctrl Pts',(3.87986928011504,66.4605263157895,3.87986928011504));
#26603=CARTESIAN_POINT('Ctrl Pts',(2.65,66.6578947368421,4.58993464005751));
#26604=CARTESIAN_POINT('Ctrl Pts',(1.42013071988495,66.8552631578948,5.29999999999999));
#26605=CARTESIAN_POINT('Ctrl Pts',(7.62668257977345E-28,67.0526315789474,
5.29999999999999));
#26606=CARTESIAN_POINT('Ctrl Pts',(-1.42013071988495,67.25,5.29999999999999));
#26607=CARTESIAN_POINT('Ctrl Pts',(-2.65,67.4473684210527,4.58993464005752));
#26608=CARTESIAN_POINT('Ctrl Pts',(-3.87986928011504,67.6447368421053,3.87986928011504));
#26609=CARTESIAN_POINT('Ctrl Pts',(-4.58993464005752,67.8421052631579,2.65));
#26610=CARTESIAN_POINT('Ctrl Pts',(-5.29999999999999,68.0394736842105,1.42013071988495));
#26611=CARTESIAN_POINT('Ctrl Pts',(-5.29999999999999,68.2368421052632,3.24531401774127E-16));
#26612=CARTESIAN_POINT('Ctrl Pts',(-5.29999999999999,68.4342105263158,-1.42013071988495));
#26613=CARTESIAN_POINT('Ctrl Pts',(-4.58993464005752,68.6315789473684,-2.65));
#26614=CARTESIAN_POINT('Ctrl Pts',(-3.87986928011504,68.828947368421,-3.87986928011504));
#26615=CARTESIAN_POINT('Ctrl Pts',(-2.65,69.0263157894736,-4.58993464005752));
#26616=CARTESIAN_POINT('Ctrl Pts',(-1.42013071988495,69.2236842105263,-5.29999999999999));
#26617=CARTESIAN_POINT('Ctrl Pts',(-6.49062803547369E-16,69.4210526315789,
-5.3));
#26618=CARTESIAN_POINT('Ctrl Pts',(1.42013071988495,69.6184210526315,-5.29999999999999));
#26619=CARTESIAN_POINT('Ctrl Pts',(2.65,69.8157894736841,-4.58993464005752));
#26620=CARTESIAN_POINT('Ctrl Pts',(3.87986928011504,70.0131578947368,-3.87986928011504));
#26621=CARTESIAN_POINT('Ctrl Pts',(4.58993464005752,70.2105263157894,-2.65));
#26622=CARTESIAN_POINT('Ctrl Pts',(5.29999999999999,70.4078947368421,-1.42013071988495));
#26623=CARTESIAN_POINT('Ctrl Pts',(5.29999999999999,70.6052631578947,-9.73594205322067E-16));
#26624=CARTESIAN_POINT('Ctrl Pts',(5.29999999999999,70.8026315789473,1.42013071988494));
#26625=CARTESIAN_POINT('Ctrl Pts',(4.58993464005752,71.,2.64999999999999));
#26626=CARTESIAN_POINT('Ctrl Pts',(3.87986928011504,71.1973684210527,3.87986928011504));
#26627=CARTESIAN_POINT('Ctrl Pts',(2.65,71.3947368421053,4.58993464005752));
#26628=CARTESIAN_POINT('Ctrl Pts',(1.42013071988495,71.5921052631579,5.29999999999999));
#26629=CARTESIAN_POINT('Ctrl Pts',(8.11201692575904E-28,71.7894736842105,
5.29999999999999));
#26630=CARTESIAN_POINT('Ctrl Pts',(-1.42013071988495,71.9868421052632,5.29999999999999));
#26631=CARTESIAN_POINT('Ctrl Pts',(-2.65,72.1842105263158,4.58993464005752));
#26632=CARTESIAN_POINT('Ctrl Pts',(-3.87986928011504,72.3815789473684,3.87986928011504));
#26633=CARTESIAN_POINT('Ctrl Pts',(-4.58993464005752,72.578947368421,2.65));
#26634=CARTESIAN_POINT('Ctrl Pts',(-5.29999999999999,72.7763157894737,1.42013071988495));
#26635=CARTESIAN_POINT('Ctrl Pts',(-5.29999999999999,72.9736842105263,3.24531401773979E-16));
#26636=CARTESIAN_POINT('Ctrl Pts',(-5.29999999999999,73.171052631579,-1.42013071988495));
#26637=CARTESIAN_POINT('Ctrl Pts',(-4.58993464005752,73.3684210526315,-2.64999999999999));
#26638=CARTESIAN_POINT('Ctrl Pts',(-3.87986928011504,73.5657894736842,-3.87986928011504));
#26639=CARTESIAN_POINT('Ctrl Pts',(-2.65,73.7631578947367,-4.58993464005752));
#26640=CARTESIAN_POINT('Ctrl Pts',(-1.42013071988495,73.9605263157894,-5.29999999999999));
#26641=CARTESIAN_POINT('Ctrl Pts',(-6.49062803547313E-16,74.157894736842,
-5.29999999999999));
#26642=CARTESIAN_POINT('Ctrl Pts',(1.42013071988495,74.3552631578946,-5.29999999999999));
#26643=CARTESIAN_POINT('Ctrl Pts',(2.65,74.5526315789473,-4.58993464005752));
#26644=CARTESIAN_POINT('Ctrl Pts',(3.87986928011504,74.75,-3.87986928011504));
#26645=CARTESIAN_POINT('Ctrl Pts',(4.58993464005752,74.9473684210526,-2.65));
#26646=CARTESIAN_POINT('Ctrl Pts',(5.29999999999999,75.1447368421053,-1.42013071988495));
#26647=CARTESIAN_POINT('Ctrl Pts',(5.29999999999999,75.3421052631579,-9.73594205322067E-16));
#26648=CARTESIAN_POINT('Ctrl Pts',(5.29999999999999,75.5394736842105,1.42013071988495));
#26649=CARTESIAN_POINT('Ctrl Pts',(4.58993464005752,75.7368421052631,2.64999999999999));
#26650=CARTESIAN_POINT('Ctrl Pts',(3.87986928011504,75.9342105263158,3.87986928011504));
#26651=CARTESIAN_POINT('Ctrl Pts',(2.65,76.1315789473684,4.58993464005751));
#26652=CARTESIAN_POINT('Ctrl Pts',(1.42013071988495,76.3289473684211,5.29999999999999));
#26653=CARTESIAN_POINT('Ctrl Pts',(8.70135148874153E-28,76.5263157894737,
5.29999999999999));
#26654=CARTESIAN_POINT('Ctrl Pts',(-1.42013071988495,76.7236842105263,5.29999999999999));
#26655=CARTESIAN_POINT('Ctrl Pts',(-2.65,76.921052631579,4.58993464005751));
#26656=CARTESIAN_POINT('Ctrl Pts',(-3.87986928011504,77.1184210526316,3.87986928011504));
#26657=CARTESIAN_POINT('Ctrl Pts',(-4.58993464005752,77.3157894736842,2.65));
#26658=CARTESIAN_POINT('Ctrl Pts',(-5.29999999999999,77.5131578947368,1.42013071988495));
#26659=CARTESIAN_POINT('Ctrl Pts',(-5.29999999999999,77.7105263157894,3.24531401773979E-16));
#26660=CARTESIAN_POINT('Ctrl Pts',(-5.29999999999999,77.9078947368421,-1.42013071988495));
#26661=CARTESIAN_POINT('Ctrl Pts',(-4.58993464005752,78.1052631578947,-2.64999999999999));
#26662=CARTESIAN_POINT('Ctrl Pts',(-3.87986928011504,78.3026315789474,-3.87986928011504));
#26663=CARTESIAN_POINT('Ctrl Pts',(-2.65,78.5,-4.58993464005752));
#26664=CARTESIAN_POINT('Ctrl Pts',(-1.42013071988495,78.6973684210526,-5.29999999999999));
#26665=CARTESIAN_POINT('Ctrl Pts',(-6.49062803547253E-16,78.8947368421053,
-5.29999999999999));
#26666=CARTESIAN_POINT('Ctrl Pts',(1.42013071988495,79.0921052631579,-5.29999999999999));
#26667=CARTESIAN_POINT('Ctrl Pts',(2.65,79.2894736842105,-4.58993464005752));
#26668=CARTESIAN_POINT('Ctrl Pts',(3.87986928011504,79.4868421052631,-3.87986928011504));
#26669=CARTESIAN_POINT('Ctrl Pts',(4.58993464005752,79.6842105263158,-2.65));
#26670=CARTESIAN_POINT('Ctrl Pts',(5.29999999999999,79.8815789473684,-1.42013071988495));
#26671=CARTESIAN_POINT('Ctrl Pts',(5.29999999999999,80.0789473684211,-9.73594205322067E-16));
#26672=CARTESIAN_POINT('Ctrl Pts',(5.29999999999999,80.2763157894737,1.42013071988495));
#26673=CARTESIAN_POINT('Ctrl Pts',(4.58993464005752,80.4736842105263,2.64999999999999));
#26674=CARTESIAN_POINT('Ctrl Pts',(3.87986928011504,80.671052631579,3.87986928011504));
#26675=CARTESIAN_POINT('Ctrl Pts',(2.65,80.8684210526316,4.58993464005752));
#26676=CARTESIAN_POINT('Ctrl Pts',(1.42013071988495,81.0657894736842,5.29999999999999));
#26677=CARTESIAN_POINT('Ctrl Pts',(9.22135257372608E-28,81.2631578947368,
5.29999999999999));
#26678=CARTESIAN_POINT('Ctrl Pts',(-1.42013071988495,81.4605263157895,5.29999999999999));
#26679=CARTESIAN_POINT('Ctrl Pts',(-2.65,81.6578947368421,4.58993464005752));
#26680=CARTESIAN_POINT('Ctrl Pts',(-3.87986928011504,81.8552631578948,3.87986928011504));
#26681=CARTESIAN_POINT('Ctrl Pts',(-4.58993464005752,82.0526315789474,2.65));
#26682=CARTESIAN_POINT('Ctrl Pts',(-5.29999999999999,82.25,1.42013071988495));
#26683=CARTESIAN_POINT('Ctrl Pts',(-5.29999999999999,82.4473684210526,3.24531401773979E-16));
#26684=CARTESIAN_POINT('Ctrl Pts',(-5.29999999999999,82.6447368421053,-1.42013071988495));
#26685=CARTESIAN_POINT('Ctrl Pts',(-4.58993464005752,82.8421052631579,-2.65));
#26686=CARTESIAN_POINT('Ctrl Pts',(-3.87986928011504,83.0394736842105,-3.87986928011504));
#26687=CARTESIAN_POINT('Ctrl Pts',(-2.65,83.2368421052631,-4.58993464005752));
#26688=CARTESIAN_POINT('Ctrl Pts',(-1.42013071988495,83.4342105263157,-5.29999999999999));
#26689=CARTESIAN_POINT('Ctrl Pts',(-6.49062803547209E-16,83.6315789473684,
-5.3));
#26690=CARTESIAN_POINT('Ctrl Pts',(1.42013071988495,83.828947368421,-5.29999999999999));
#26691=CARTESIAN_POINT('Ctrl Pts',(2.65,84.0263157894736,-4.58993464005752));
#26692=CARTESIAN_POINT('Ctrl Pts',(3.87986928011504,84.2236842105263,-3.87986928011504));
#26693=CARTESIAN_POINT('Ctrl Pts',(4.58993464005752,84.4210526315789,-2.65));
#26694=CARTESIAN_POINT('Ctrl Pts',(5.29999999999999,84.6184210526316,-1.42013071988495));
#26695=CARTESIAN_POINT('Ctrl Pts',(5.29999999999999,84.8157894736842,-9.73594205321179E-16));
#26696=CARTESIAN_POINT('Ctrl Pts',(5.29999999999999,85.0131578947368,1.42013071988495));
#26697=CARTESIAN_POINT('Ctrl Pts',(4.58993464005752,85.2105263157895,2.64999999999999));
#26698=CARTESIAN_POINT('Ctrl Pts',(3.87986928011504,85.4078947368421,3.87986928011504));
#26699=CARTESIAN_POINT('Ctrl Pts',(2.65,85.6052631578948,4.58993464005751));
#26700=CARTESIAN_POINT('Ctrl Pts',(1.42013071988495,85.8026315789474,5.29999999999999));
#26701=CARTESIAN_POINT('Ctrl Pts',(9.70668691971167E-28,86.0000000000001,
5.29999999999999));
#26702=CARTESIAN_POINT('Ctrl Pts',(2.77333911991762E-29,0.,5.29999999999999));
#26703=CARTESIAN_POINT('Ctrl Pts',(-1.42013071988495,0.197368421052638,
5.29999999999998));
#26704=CARTESIAN_POINT('Ctrl Pts',(-2.65,0.394736842105281,4.58993464005751));
#26705=CARTESIAN_POINT('Ctrl Pts',(-3.87986928011504,0.592105263157915,
3.87986928011505));
#26706=CARTESIAN_POINT('Ctrl Pts',(-4.58993464005751,0.789473684210562,
2.65));
#26707=CARTESIAN_POINT('Ctrl Pts',(-5.29999999999999,0.986842105263191,
1.42013071988495));
#26708=CARTESIAN_POINT('Ctrl Pts',(-5.29999999999999,1.18421052631579,3.24531401774024E-16));
#26709=CARTESIAN_POINT('Ctrl Pts',(-5.29999999999999,1.38157894736841,-1.42013071988495));
#26710=CARTESIAN_POINT('Ctrl Pts',(-4.58993464005751,1.57894736842107,-2.64999999999999));
#26711=CARTESIAN_POINT('Ctrl Pts',(-3.87986928011504,1.77631578947369,-3.87986928011504));
#26712=CARTESIAN_POINT('Ctrl Pts',(-2.65,1.97368421052629,-4.58993464005751));
#26713=CARTESIAN_POINT('Ctrl Pts',(-1.42013071988495,2.17105263157891,-5.29999999999999));
#26714=CARTESIAN_POINT('Ctrl Pts',(-6.49062803548097E-16,2.36842105263158,
-5.29999999999999));
#26715=CARTESIAN_POINT('Ctrl Pts',(1.42013071988495,2.56578947368418,-5.29999999999999));
#26716=CARTESIAN_POINT('Ctrl Pts',(2.64999999999999,2.7631578947368,-4.58993464005751));
#26717=CARTESIAN_POINT('Ctrl Pts',(3.87986928011504,2.96052631578946,-3.87986928011505));
#26718=CARTESIAN_POINT('Ctrl Pts',(4.58993464005751,3.15789473684208,-2.65));
#26719=CARTESIAN_POINT('Ctrl Pts',(5.29999999999999,3.35526315789473,-1.42013071988495));
#26720=CARTESIAN_POINT('Ctrl Pts',(5.29999999999999,3.55263157894736,-9.73594205321085E-16));
#26721=CARTESIAN_POINT('Ctrl Pts',(5.29999999999999,3.75000000000001,1.42013071988494));
#26722=CARTESIAN_POINT('Ctrl Pts',(4.58993464005752,3.94736842105264,2.64999999999999));
#26723=CARTESIAN_POINT('Ctrl Pts',(3.87986928011505,4.14473684210529,3.87986928011504));
#26724=CARTESIAN_POINT('Ctrl Pts',(2.65,4.34210526315792,4.58993464005751));
#26725=CARTESIAN_POINT('Ctrl Pts',(1.42013071988495,4.53947368421056,5.29999999999998));
#26726=CARTESIAN_POINT('Ctrl Pts',(8.32001735975286E-29,4.73684210526315,
5.29999999999999));
#26727=CARTESIAN_POINT('Ctrl Pts',(-1.42013071988495,4.93421052631578,5.29999999999999));
#26728=CARTESIAN_POINT('Ctrl Pts',(-2.65,5.13157894736843,4.58993464005751));
#26729=CARTESIAN_POINT('Ctrl Pts',(-3.87986928011504,5.32894736842106,3.87986928011505));
#26730=CARTESIAN_POINT('Ctrl Pts',(-4.58993464005751,5.52631578947371,2.65));
#26731=CARTESIAN_POINT('Ctrl Pts',(-5.29999999999999,5.72368421052634,1.42013071988495));
#26732=CARTESIAN_POINT('Ctrl Pts',(-5.29999999999999,5.92105263157894,3.24531401774024E-16));
#26733=CARTESIAN_POINT('Ctrl Pts',(-5.29999999999999,6.11842105263156,-1.42013071988495));
#26734=CARTESIAN_POINT('Ctrl Pts',(-4.58993464005751,6.31578947368422,-2.64999999999999));
#26735=CARTESIAN_POINT('Ctrl Pts',(-3.87986928011504,6.51315789473683,-3.87986928011504));
#26736=CARTESIAN_POINT('Ctrl Pts',(-2.65,6.71052631578944,-4.58993464005751));
#26737=CARTESIAN_POINT('Ctrl Pts',(-1.42013071988495,6.90789473684211,-5.29999999999999));
#26738=CARTESIAN_POINT('Ctrl Pts',(-6.49062803548043E-16,7.10526315789473,
-5.29999999999999));
#26739=CARTESIAN_POINT('Ctrl Pts',(1.42013071988495,7.30263157894733,-5.29999999999999));
#26740=CARTESIAN_POINT('Ctrl Pts',(2.64999999999999,7.50000000000001,-4.58993464005751));
#26741=CARTESIAN_POINT('Ctrl Pts',(3.87986928011504,7.69736842105261,-3.87986928011505));
#26742=CARTESIAN_POINT('Ctrl Pts',(4.58993464005751,7.89473684210523,-2.65));
#26743=CARTESIAN_POINT('Ctrl Pts',(5.29999999999999,8.09210526315788,-1.42013071988495));
#26744=CARTESIAN_POINT('Ctrl Pts',(5.29999999999999,8.28947368421051,-9.73594205321085E-16));
#26745=CARTESIAN_POINT('Ctrl Pts',(5.29999999999999,8.48684210526316,1.42013071988495));
#26746=CARTESIAN_POINT('Ctrl Pts',(4.58993464005752,8.68421052631579,2.64999999999999));
#26747=CARTESIAN_POINT('Ctrl Pts',(3.87986928011505,8.88157894736843,3.87986928011504));
#26748=CARTESIAN_POINT('Ctrl Pts',(2.65,9.07894736842108,4.58993464005751));
#26749=CARTESIAN_POINT('Ctrl Pts',(1.42013071988495,9.27631578947371,5.29999999999999));
#26750=CARTESIAN_POINT('Ctrl Pts',(1.35585468084861E-28,9.47368421052636,
5.3));
#26751=CARTESIAN_POINT('Ctrl Pts',(-1.42013071988495,9.67105263157899,5.29999999999998));
#26752=CARTESIAN_POINT('Ctrl Pts',(-2.65,9.86842105263158,4.58993464005751));
#26753=CARTESIAN_POINT('Ctrl Pts',(-3.87986928011504,10.0657894736842,3.87986928011504));
#26754=CARTESIAN_POINT('Ctrl Pts',(-4.58993464005751,10.2631578947369,2.65));
#26755=CARTESIAN_POINT('Ctrl Pts',(-5.29999999999999,10.4605263157895,1.42013071988495));
#26756=CARTESIAN_POINT('Ctrl Pts',(-5.29999999999999,10.6578947368421,3.24531401772841E-16));
#26757=CARTESIAN_POINT('Ctrl Pts',(-5.29999999999999,10.8552631578948,-1.42013071988495));
#26758=CARTESIAN_POINT('Ctrl Pts',(-4.58993464005751,11.0526315789474,-2.64999999999999));
#26759=CARTESIAN_POINT('Ctrl Pts',(-3.87986928011504,11.25,-3.87986928011504));
#26760=CARTESIAN_POINT('Ctrl Pts',(-2.65,11.4473684210526,-4.58993464005751));
#26761=CARTESIAN_POINT('Ctrl Pts',(-1.42013071988495,11.6447368421052,-5.29999999999999));
#26762=CARTESIAN_POINT('Ctrl Pts',(-6.49062803547995E-16,11.8421052631579,
-5.29999999999999));
#26763=CARTESIAN_POINT('Ctrl Pts',(1.42013071988495,12.0394736842105,-5.29999999999999));
#26764=CARTESIAN_POINT('Ctrl Pts',(2.64999999999999,12.2368421052632,-4.58993464005751));
#26765=CARTESIAN_POINT('Ctrl Pts',(3.87986928011504,12.4342105263158,-3.87986928011505));
#26766=CARTESIAN_POINT('Ctrl Pts',(4.58993464005751,12.6315789473684,-2.65));
#26767=CARTESIAN_POINT('Ctrl Pts',(5.29999999999999,12.828947368421,-1.42013071988495));
#26768=CARTESIAN_POINT('Ctrl Pts',(5.29999999999999,13.0263157894737,-9.73594205322072E-16));
#26769=CARTESIAN_POINT('Ctrl Pts',(5.29999999999999,13.2236842105263,1.42013071988495));
#26770=CARTESIAN_POINT('Ctrl Pts',(4.58993464005752,13.4210526315789,2.64999999999999));
#26771=CARTESIAN_POINT('Ctrl Pts',(3.87986928011505,13.6184210526316,3.87986928011504));
#26772=CARTESIAN_POINT('Ctrl Pts',(2.65,13.8157894736842,4.58993464005751));
#26773=CARTESIAN_POINT('Ctrl Pts',(1.42013071988495,14.0131578947369,5.29999999999998));
#26774=CARTESIAN_POINT('Ctrl Pts',(1.84889274661175E-28,14.2105263157895,
5.3));
#26775=CARTESIAN_POINT('Ctrl Pts',(-1.42013071988495,14.4078947368421,5.29999999999999));
#26776=CARTESIAN_POINT('Ctrl Pts',(-2.65,14.6052631578947,4.58993464005751));
#26777=CARTESIAN_POINT('Ctrl Pts',(-3.87986928011504,14.8026315789474,3.87986928011504));
#26778=CARTESIAN_POINT('Ctrl Pts',(-4.58993464005751,15.,2.65));
#26779=CARTESIAN_POINT('Ctrl Pts',(-5.29999999999999,15.1973684210526,1.42013071988495));
#26780=CARTESIAN_POINT('Ctrl Pts',(-5.29999999999999,15.3947368421052,3.24531401774024E-16));
#26781=CARTESIAN_POINT('Ctrl Pts',(-5.29999999999999,15.5921052631579,-1.42013071988495));
#26782=CARTESIAN_POINT('Ctrl Pts',(-4.58993464005751,15.7894736842105,-2.64999999999999));
#26783=CARTESIAN_POINT('Ctrl Pts',(-3.87986928011504,15.9868421052631,-3.87986928011504));
#26784=CARTESIAN_POINT('Ctrl Pts',(-2.65,16.1842105263157,-4.58993464005751));
#26785=CARTESIAN_POINT('Ctrl Pts',(-1.42013071988495,16.3815789473684,-5.29999999999999));
#26786=CARTESIAN_POINT('Ctrl Pts',(-6.49062803547949E-16,16.578947368421,
-5.29999999999999));
#26787=CARTESIAN_POINT('Ctrl Pts',(1.42013071988495,16.7763157894737,-5.29999999999999));
#26788=CARTESIAN_POINT('Ctrl Pts',(2.64999999999999,16.9736842105263,-4.58993464005751));
#26789=CARTESIAN_POINT('Ctrl Pts',(3.87986928011504,17.171052631579,-3.87986928011505));
#26790=CARTESIAN_POINT('Ctrl Pts',(4.58993464005751,17.3684210526316,-2.65));
#26791=CARTESIAN_POINT('Ctrl Pts',(5.29999999999999,17.5657894736842,-1.42013071988495));
#26792=CARTESIAN_POINT('Ctrl Pts',(5.29999999999999,17.7631578947368,-9.73594205322269E-16));
#26793=CARTESIAN_POINT('Ctrl Pts',(5.29999999999999,17.9605263157895,1.42013071988494));
#26794=CARTESIAN_POINT('Ctrl Pts',(4.58993464005752,18.1578947368421,2.64999999999999));
#26795=CARTESIAN_POINT('Ctrl Pts',(3.87986928011505,18.3552631578947,3.87986928011504));
#26796=CARTESIAN_POINT('Ctrl Pts',(2.65,18.5526315789474,4.58993464005751));
#26797=CARTESIAN_POINT('Ctrl Pts',(1.42013071988495,18.75,5.29999999999998));
#26798=CARTESIAN_POINT('Ctrl Pts',(2.31111593326468E-28,18.9473684210527,
5.3));
#26799=CARTESIAN_POINT('Ctrl Pts',(-1.42013071988495,19.1447368421053,5.29999999999999));
#26800=CARTESIAN_POINT('Ctrl Pts',(-2.65,19.3421052631579,4.58993464005751));
#26801=CARTESIAN_POINT('Ctrl Pts',(-3.87986928011504,19.5394736842105,3.87986928011504));
#26802=CARTESIAN_POINT('Ctrl Pts',(-4.58993464005751,19.7368421052632,2.65));
#26803=CARTESIAN_POINT('Ctrl Pts',(-5.29999999999999,19.9342105263158,1.42013071988495));
#26804=CARTESIAN_POINT('Ctrl Pts',(-5.29999999999999,20.1315789473684,3.24531401774221E-16));
#26805=CARTESIAN_POINT('Ctrl Pts',(-5.29999999999999,20.328947368421,-1.42013071988495));
#26806=CARTESIAN_POINT('Ctrl Pts',(-4.58993464005751,20.5263157894737,-2.64999999999999));
#26807=CARTESIAN_POINT('Ctrl Pts',(-3.87986928011504,20.7236842105263,-3.87986928011504));
#26808=CARTESIAN_POINT('Ctrl Pts',(-2.65,20.921052631579,-4.58993464005751));
#26809=CARTESIAN_POINT('Ctrl Pts',(-1.42013071988495,21.1184210526315,-5.29999999999999));
#26810=CARTESIAN_POINT('Ctrl Pts',(-6.49062803547894E-16,21.3157894736842,
-5.29999999999999));
#26811=CARTESIAN_POINT('Ctrl Pts',(1.42013071988495,21.5131578947368,-5.29999999999999));
#26812=CARTESIAN_POINT('Ctrl Pts',(2.64999999999999,21.7105263157895,-4.58993464005751));
#26813=CARTESIAN_POINT('Ctrl Pts',(3.87986928011504,21.9078947368421,-3.87986928011505));
#26814=CARTESIAN_POINT('Ctrl Pts',(4.58993464005751,22.1052631578947,-2.65));
#26815=CARTESIAN_POINT('Ctrl Pts',(5.29999999999999,22.3026315789474,-1.42013071988495));
#26816=CARTESIAN_POINT('Ctrl Pts',(5.29999999999999,22.5,-9.73594205320888E-16));
#26817=CARTESIAN_POINT('Ctrl Pts',(5.29999999999999,22.6973684210527,1.42013071988495));
#26818=CARTESIAN_POINT('Ctrl Pts',(4.58993464005752,22.8947368421052,2.64999999999999));
#26819=CARTESIAN_POINT('Ctrl Pts',(3.87986928011505,23.0921052631579,3.87986928011504));
#26820=CARTESIAN_POINT('Ctrl Pts',(2.65,23.2894736842105,4.58993464005751));
#26821=CARTESIAN_POINT('Ctrl Pts',(1.42013071988495,23.4868421052631,5.29999999999999));
#26822=CARTESIAN_POINT('Ctrl Pts',(2.95822839457879E-28,23.6842105263158,
5.3));
#26823=CARTESIAN_POINT('Ctrl Pts',(-1.42013071988495,23.8815789473684,5.29999999999998));
#26824=CARTESIAN_POINT('Ctrl Pts',(-2.65,24.0789473684211,4.58993464005751));
#26825=CARTESIAN_POINT('Ctrl Pts',(-3.87986928011504,24.2763157894737,3.87986928011504));
#26826=CARTESIAN_POINT('Ctrl Pts',(-4.58993464005751,24.4736842105263,2.65));
#26827=CARTESIAN_POINT('Ctrl Pts',(-5.29999999999999,24.671052631579,1.42013071988495));
#26828=CARTESIAN_POINT('Ctrl Pts',(-5.29999999999999,24.8684210526316,3.24531401774024E-16));
#26829=CARTESIAN_POINT('Ctrl Pts',(-5.29999999999999,25.0657894736842,-1.42013071988495));
#26830=CARTESIAN_POINT('Ctrl Pts',(-4.58993464005751,25.2631578947368,-2.64999999999999));
#26831=CARTESIAN_POINT('Ctrl Pts',(-3.87986928011504,25.4605263157895,-3.87986928011504));
#26832=CARTESIAN_POINT('Ctrl Pts',(-2.65,25.6578947368421,-4.58993464005751));
#26833=CARTESIAN_POINT('Ctrl Pts',(-1.42013071988495,25.8552631578947,-5.29999999999999));
#26834=CARTESIAN_POINT('Ctrl Pts',(-6.49062803547834E-16,26.0526315789473,
-5.29999999999999));
#26835=CARTESIAN_POINT('Ctrl Pts',(1.42013071988495,26.25,-5.29999999999999));
#26836=CARTESIAN_POINT('Ctrl Pts',(2.64999999999999,26.4473684210526,-4.58993464005752));
#26837=CARTESIAN_POINT('Ctrl Pts',(3.87986928011504,26.6447368421052,-3.87986928011505));
#26838=CARTESIAN_POINT('Ctrl Pts',(4.58993464005751,26.8421052631579,-2.65));
#26839=CARTESIAN_POINT('Ctrl Pts',(5.29999999999999,27.0394736842105,-1.42013071988495));
#26840=CARTESIAN_POINT('Ctrl Pts',(5.29999999999999,27.2368421052632,-9.73594205320888E-16));
#26841=CARTESIAN_POINT('Ctrl Pts',(5.29999999999999,27.4342105263158,1.42013071988495));
#26842=CARTESIAN_POINT('Ctrl Pts',(4.58993464005752,27.6315789473685,2.64999999999999));
#26843=CARTESIAN_POINT('Ctrl Pts',(3.87986928011505,27.8289473684211,3.87986928011504));
#26844=CARTESIAN_POINT('Ctrl Pts',(2.65,28.0263157894737,4.58993464005751));
#26845=CARTESIAN_POINT('Ctrl Pts',(1.42013071988495,28.2236842105264,5.29999999999998));
#26846=CARTESIAN_POINT('Ctrl Pts',(3.42045158123173E-28,28.421052631579,
5.3));
#26847=CARTESIAN_POINT('Ctrl Pts',(-1.42013071988495,28.6184210526316,5.29999999999999));
#26848=CARTESIAN_POINT('Ctrl Pts',(-2.65,28.8157894736842,4.58993464005751));
#26849=CARTESIAN_POINT('Ctrl Pts',(-3.87986928011504,29.0131578947368,3.87986928011504));
#26850=CARTESIAN_POINT('Ctrl Pts',(-4.58993464005751,29.2105263157895,2.65));
#26851=CARTESIAN_POINT('Ctrl Pts',(-5.29999999999999,29.4078947368421,1.42013071988495));
#26852=CARTESIAN_POINT('Ctrl Pts',(-5.29999999999999,29.6052631578947,3.24531401774024E-16));
#26853=CARTESIAN_POINT('Ctrl Pts',(-5.29999999999999,29.8026315789473,-1.42013071988495));
#26854=CARTESIAN_POINT('Ctrl Pts',(-4.58993464005751,30.,-2.64999999999999));
#26855=CARTESIAN_POINT('Ctrl Pts',(-3.87986928011504,30.1973684210526,-3.87986928011504));
#26856=CARTESIAN_POINT('Ctrl Pts',(-2.65,30.3947368421053,-4.58993464005751));
#26857=CARTESIAN_POINT('Ctrl Pts',(-1.42013071988495,30.5921052631579,-5.29999999999999));
#26858=CARTESIAN_POINT('Ctrl Pts',(-6.49062803547783E-16,30.7894736842105,
-5.29999999999999));
#26859=CARTESIAN_POINT('Ctrl Pts',(1.42013071988495,30.9868421052631,-5.29999999999999));
#26860=CARTESIAN_POINT('Ctrl Pts',(2.64999999999999,31.1842105263158,-4.58993464005752));
#26861=CARTESIAN_POINT('Ctrl Pts',(3.87986928011504,31.3815789473684,-3.87986928011505));
#26862=CARTESIAN_POINT('Ctrl Pts',(4.58993464005751,31.578947368421,-2.65));
#26863=CARTESIAN_POINT('Ctrl Pts',(5.29999999999999,31.7763157894737,-1.42013071988495));
#26864=CARTESIAN_POINT('Ctrl Pts',(5.29999999999999,31.9736842105263,-9.73594205321085E-16));
#26865=CARTESIAN_POINT('Ctrl Pts',(5.29999999999999,32.1710526315789,1.42013071988495));
#26866=CARTESIAN_POINT('Ctrl Pts',(4.58993464005752,32.3684210526316,2.64999999999999));
#26867=CARTESIAN_POINT('Ctrl Pts',(3.87986928011505,32.5657894736842,3.87986928011504));
#26868=CARTESIAN_POINT('Ctrl Pts',(2.65,32.7631578947368,4.58993464005751));
#26869=CARTESIAN_POINT('Ctrl Pts',(1.42013071988495,32.9605263157895,5.29999999999999));
#26870=CARTESIAN_POINT('Ctrl Pts',(3.88267476788467E-28,33.1578947368421,
5.3));
#26871=CARTESIAN_POINT('Ctrl Pts',(-1.42013071988495,33.3552631578948,5.29999999999998));
#26872=CARTESIAN_POINT('Ctrl Pts',(-2.65,33.5526315789474,4.58993464005751));
#26873=CARTESIAN_POINT('Ctrl Pts',(-3.87986928011504,33.75,3.87986928011505));
#26874=CARTESIAN_POINT('Ctrl Pts',(-4.58993464005751,33.9473684210526,2.65));
#26875=CARTESIAN_POINT('Ctrl Pts',(-5.29999999999999,34.1447368421052,1.42013071988495));
#26876=CARTESIAN_POINT('Ctrl Pts',(-5.29999999999999,34.3421052631579,3.24531401774024E-16));
#26877=CARTESIAN_POINT('Ctrl Pts',(-5.29999999999999,34.5394736842105,-1.42013071988495));
#26878=CARTESIAN_POINT('Ctrl Pts',(-4.58993464005751,34.7368421052631,-2.65));
#26879=CARTESIAN_POINT('Ctrl Pts',(-3.87986928011504,34.9342105263158,-3.87986928011504));
#26880=CARTESIAN_POINT('Ctrl Pts',(-2.65,35.1315789473684,-4.58993464005751));
#26881=CARTESIAN_POINT('Ctrl Pts',(-1.42013071988495,35.328947368421,-5.29999999999999));
#26882=CARTESIAN_POINT('Ctrl Pts',(-6.49062803547736E-16,35.5263157894737,
-5.29999999999999));
#26883=CARTESIAN_POINT('Ctrl Pts',(1.42013071988495,35.7236842105263,-5.29999999999999));
#26884=CARTESIAN_POINT('Ctrl Pts',(2.64999999999999,35.9210526315789,-4.58993464005752));
#26885=CARTESIAN_POINT('Ctrl Pts',(3.87986928011504,36.1184210526315,-3.87986928011505));
#26886=CARTESIAN_POINT('Ctrl Pts',(4.58993464005751,36.3157894736842,-2.65));
#26887=CARTESIAN_POINT('Ctrl Pts',(5.29999999999999,36.5131578947368,-1.42013071988495));
#26888=CARTESIAN_POINT('Ctrl Pts',(5.29999999999999,36.7105263157895,-9.73594205322072E-16));
#26889=CARTESIAN_POINT('Ctrl Pts',(5.29999999999999,36.9078947368421,1.42013071988495));
#26890=CARTESIAN_POINT('Ctrl Pts',(4.58993464005752,37.1052631578948,2.64999999999999));
#26891=CARTESIAN_POINT('Ctrl Pts',(3.87986928011505,37.3026315789473,3.87986928011504));
#26892=CARTESIAN_POINT('Ctrl Pts',(2.65,37.5,4.58993464005751));
#26893=CARTESIAN_POINT('Ctrl Pts',(1.42013071988495,37.6973684210526,5.29999999999998));
#26894=CARTESIAN_POINT('Ctrl Pts',(4.42193515231309E-28,37.8947368421053,
5.29999999999999));
#26895=CARTESIAN_POINT('Ctrl Pts',(-1.42013071988495,38.0921052631579,5.29999999999999));
#26896=CARTESIAN_POINT('Ctrl Pts',(-2.65,38.2894736842105,4.58993464005752));
#26897=CARTESIAN_POINT('Ctrl Pts',(-3.87986928011504,38.4868421052632,3.87986928011504));
#26898=CARTESIAN_POINT('Ctrl Pts',(-4.58993464005751,38.6842105263158,2.65));
#26899=CARTESIAN_POINT('Ctrl Pts',(-5.29999999999999,38.8815789473684,1.42013071988495));
#26900=CARTESIAN_POINT('Ctrl Pts',(-5.29999999999999,39.078947368421,3.24531401774024E-16));
#26901=CARTESIAN_POINT('Ctrl Pts',(-5.29999999999999,39.2763157894737,-1.42013071988495));
#26902=CARTESIAN_POINT('Ctrl Pts',(-4.58993464005751,39.4736842105263,-2.64999999999999));
#26903=CARTESIAN_POINT('Ctrl Pts',(-3.87986928011504,39.6710526315789,-3.87986928011504));
#26904=CARTESIAN_POINT('Ctrl Pts',(-2.65,39.8684210526316,-4.58993464005751));
#26905=CARTESIAN_POINT('Ctrl Pts',(-1.42013071988495,40.0657894736842,-5.29999999999999));
#26906=CARTESIAN_POINT('Ctrl Pts',(-6.49062803547683E-16,40.2631578947368,
-5.29999999999999));
#26907=CARTESIAN_POINT('Ctrl Pts',(1.42013071988495,40.4605263157895,-5.29999999999999));
#26908=CARTESIAN_POINT('Ctrl Pts',(2.64999999999999,40.6578947368421,-4.58993464005752));
#26909=CARTESIAN_POINT('Ctrl Pts',(3.87986928011504,40.8552631578947,-3.87986928011505));
#26910=CARTESIAN_POINT('Ctrl Pts',(4.58993464005751,41.0526315789473,-2.65));
#26911=CARTESIAN_POINT('Ctrl Pts',(5.29999999999999,41.25,-1.42013071988495));
#26912=CARTESIAN_POINT('Ctrl Pts',(5.29999999999999,41.4473684210526,-9.73594205322072E-16));
#26913=CARTESIAN_POINT('Ctrl Pts',(5.29999999999999,41.6447368421053,1.42013071988495));
#26914=CARTESIAN_POINT('Ctrl Pts',(4.58993464005752,41.8421052631579,2.64999999999999));
#26915=CARTESIAN_POINT('Ctrl Pts',(3.87986928011505,42.0394736842106,3.87986928011504));
#26916=CARTESIAN_POINT('Ctrl Pts',(2.65,42.2368421052632,4.58993464005751));
#26917=CARTESIAN_POINT('Ctrl Pts',(1.42013071988495,42.4342105263158,5.29999999999999));
#26918=CARTESIAN_POINT('Ctrl Pts',(4.99201041585172E-28,42.6315789473684,
5.29999999999999));
#26919=CARTESIAN_POINT('Ctrl Pts',(-1.42013071988495,42.8289473684211,5.29999999999998));
#26920=CARTESIAN_POINT('Ctrl Pts',(-2.65,43.0263157894737,4.58993464005752));
#26921=CARTESIAN_POINT('Ctrl Pts',(-3.87986928011504,43.2236842105263,3.87986928011504));
#26922=CARTESIAN_POINT('Ctrl Pts',(-4.58993464005751,43.421052631579,2.65));
#26923=CARTESIAN_POINT('Ctrl Pts',(-5.29999999999999,43.6184210526316,1.42013071988495));
#26924=CARTESIAN_POINT('Ctrl Pts',(-5.29999999999999,43.8157894736842,3.24531401774024E-16));
#26925=CARTESIAN_POINT('Ctrl Pts',(-5.29999999999999,44.0131578947368,-1.42013071988495));
#26926=CARTESIAN_POINT('Ctrl Pts',(-4.58993464005751,44.2105263157895,-2.64999999999999));
#26927=CARTESIAN_POINT('Ctrl Pts',(-3.87986928011504,44.4078947368421,-3.87986928011504));
#26928=CARTESIAN_POINT('Ctrl Pts',(-2.65,44.6052631578947,-4.58993464005751));
#26929=CARTESIAN_POINT('Ctrl Pts',(-1.42013071988495,44.8026315789473,-5.29999999999999));
#26930=CARTESIAN_POINT('Ctrl Pts',(-6.49062803547635E-16,45.,-5.29999999999999));
#26931=CARTESIAN_POINT('Ctrl Pts',(1.42013071988495,45.1973684210526,-5.29999999999999));
#26932=CARTESIAN_POINT('Ctrl Pts',(2.64999999999999,45.3947368421053,-4.58993464005752));
#26933=CARTESIAN_POINT('Ctrl Pts',(3.87986928011504,45.5921052631579,-3.87986928011505));
#26934=CARTESIAN_POINT('Ctrl Pts',(4.58993464005751,45.7894736842105,-2.65));
#26935=CARTESIAN_POINT('Ctrl Pts',(5.29999999999999,45.9868421052631,-1.42013071988495));
#26936=CARTESIAN_POINT('Ctrl Pts',(5.29999999999999,46.1842105263158,-9.73594205321085E-16));
#26937=CARTESIAN_POINT('Ctrl Pts',(5.29999999999999,46.3815789473684,1.42013071988495));
#26938=CARTESIAN_POINT('Ctrl Pts',(4.58993464005752,46.5789473684211,2.64999999999999));
#26939=CARTESIAN_POINT('Ctrl Pts',(3.87986928011505,46.7763157894737,3.87986928011504));
#26940=CARTESIAN_POINT('Ctrl Pts',(2.65,46.9736842105263,4.58993464005752));
#26941=CARTESIAN_POINT('Ctrl Pts',(1.42013071988495,47.1710526315789,5.29999999999999));
#26942=CARTESIAN_POINT('Ctrl Pts',(5.54667823983524E-28,47.3684210526316,
5.29999999999999));
#26943=CARTESIAN_POINT('Ctrl Pts',(-1.42013071988495,47.5657894736842,5.29999999999998));
#26944=CARTESIAN_POINT('Ctrl Pts',(-2.65,47.7631578947368,4.58993464005752));
#26945=CARTESIAN_POINT('Ctrl Pts',(-3.87986928011504,47.9605263157895,3.87986928011504));
#26946=CARTESIAN_POINT('Ctrl Pts',(-4.58993464005751,48.1578947368421,2.65));
#26947=CARTESIAN_POINT('Ctrl Pts',(-5.29999999999999,48.3552631578947,1.42013071988495));
#26948=CARTESIAN_POINT('Ctrl Pts',(-5.29999999999999,48.5526315789474,3.24531401773827E-16));
#26949=CARTESIAN_POINT('Ctrl Pts',(-5.29999999999999,48.75,-1.42013071988495));
#26950=CARTESIAN_POINT('Ctrl Pts',(-4.58993464005751,48.9473684210526,-2.64999999999999));
#26951=CARTESIAN_POINT('Ctrl Pts',(-3.87986928011504,49.1447368421053,-3.87986928011504));
#26952=CARTESIAN_POINT('Ctrl Pts',(-2.65,49.3421052631579,-4.58993464005751));
#26953=CARTESIAN_POINT('Ctrl Pts',(-1.42013071988495,49.5394736842105,-5.29999999999999));
#26954=CARTESIAN_POINT('Ctrl Pts',(-6.49062803547579E-16,49.7368421052631,
-5.29999999999999));
#26955=CARTESIAN_POINT('Ctrl Pts',(1.42013071988495,49.9342105263158,-5.29999999999999));
#26956=CARTESIAN_POINT('Ctrl Pts',(2.64999999999999,50.1315789473684,-4.58993464005752));
#26957=CARTESIAN_POINT('Ctrl Pts',(3.87986928011504,50.328947368421,-3.87986928011505));
#26958=CARTESIAN_POINT('Ctrl Pts',(4.58993464005751,50.5263157894737,-2.65));
#26959=CARTESIAN_POINT('Ctrl Pts',(5.29999999999999,50.7236842105263,-1.42013071988495));
#26960=CARTESIAN_POINT('Ctrl Pts',(5.29999999999999,50.9210526315789,-9.73594205321085E-16));
#26961=CARTESIAN_POINT('Ctrl Pts',(5.29999999999999,51.1184210526316,1.42013071988495));
#26962=CARTESIAN_POINT('Ctrl Pts',(4.58993464005752,51.3157894736842,2.64999999999999));
#26963=CARTESIAN_POINT('Ctrl Pts',(3.87986928011505,51.5131578947368,3.87986928011504));
#26964=CARTESIAN_POINT('Ctrl Pts',(2.65,51.7105263157895,4.58993464005752));
#26965=CARTESIAN_POINT('Ctrl Pts',(1.42013071988495,51.9078947368421,5.29999999999998));
#26966=CARTESIAN_POINT('Ctrl Pts',(6.00890142648818E-28,52.1052631578948,
5.29999999999999));
#26967=CARTESIAN_POINT('Ctrl Pts',(-1.42013071988495,52.3026315789474,5.29999999999999));
#26968=CARTESIAN_POINT('Ctrl Pts',(-2.65,52.5,4.58993464005752));
#26969=CARTESIAN_POINT('Ctrl Pts',(-3.87986928011504,52.6973684210526,3.87986928011504));
#26970=CARTESIAN_POINT('Ctrl Pts',(-4.58993464005751,52.8947368421053,2.65));
#26971=CARTESIAN_POINT('Ctrl Pts',(-5.29999999999999,53.0921052631579,1.42013071988495));
#26972=CARTESIAN_POINT('Ctrl Pts',(-5.29999999999999,53.2894736842105,3.245314017757E-16));
#26973=CARTESIAN_POINT('Ctrl Pts',(-5.29999999999999,53.4868421052631,-1.42013071988495));
#26974=CARTESIAN_POINT('Ctrl Pts',(-4.58993464005751,53.6842105263158,-2.64999999999999));
#26975=CARTESIAN_POINT('Ctrl Pts',(-3.87986928011504,53.8815789473684,-3.87986928011504));
#26976=CARTESIAN_POINT('Ctrl Pts',(-2.65,54.0789473684211,-4.58993464005751));
#26977=CARTESIAN_POINT('Ctrl Pts',(-1.42013071988495,54.2763157894737,-5.29999999999999));
#26978=CARTESIAN_POINT('Ctrl Pts',(-6.4906280354753E-16,54.4736842105263,
-5.29999999999999));
#26979=CARTESIAN_POINT('Ctrl Pts',(1.42013071988495,54.6710526315789,-5.29999999999999));
#26980=CARTESIAN_POINT('Ctrl Pts',(2.64999999999999,54.8684210526316,-4.58993464005752));
#26981=CARTESIAN_POINT('Ctrl Pts',(3.87986928011504,55.0657894736842,-3.87986928011505));
#26982=CARTESIAN_POINT('Ctrl Pts',(4.58993464005751,55.2631578947368,-2.65));
#26983=CARTESIAN_POINT('Ctrl Pts',(5.29999999999999,55.4605263157895,-1.42013071988495));
#26984=CARTESIAN_POINT('Ctrl Pts',(5.29999999999999,55.6578947368421,-9.73594205321578E-16));
#26985=CARTESIAN_POINT('Ctrl Pts',(5.29999999999999,55.8552631578947,1.42013071988495));
#26986=CARTESIAN_POINT('Ctrl Pts',(4.58993464005752,56.0526315789474,2.64999999999999));
#26987=CARTESIAN_POINT('Ctrl Pts',(3.87986928011505,56.25,3.87986928011504));
#26988=CARTESIAN_POINT('Ctrl Pts',(2.65,56.4473684210526,4.58993464005752));
#26989=CARTESIAN_POINT('Ctrl Pts',(1.42013071988495,56.6447368421052,5.29999999999999));
#26990=CARTESIAN_POINT('Ctrl Pts',(6.5635692504717E-28,56.8421052631579,
5.29999999999999));
#26991=CARTESIAN_POINT('Ctrl Pts',(-1.42013071988495,57.0394736842105,5.29999999999998));
#26992=CARTESIAN_POINT('Ctrl Pts',(-2.65,57.2368421052632,4.58993464005752));
#26993=CARTESIAN_POINT('Ctrl Pts',(-3.87986928011504,57.4342105263158,3.87986928011504));
#26994=CARTESIAN_POINT('Ctrl Pts',(-4.58993464005751,57.6315789473684,2.65));
#26995=CARTESIAN_POINT('Ctrl Pts',(-5.29999999999999,57.8289473684211,1.42013071988495));
#26996=CARTESIAN_POINT('Ctrl Pts',(-5.29999999999999,58.0263157894737,3.24531401775207E-16));
#26997=CARTESIAN_POINT('Ctrl Pts',(-5.29999999999999,58.2236842105263,-1.42013071988495));
#26998=CARTESIAN_POINT('Ctrl Pts',(-4.58993464005751,58.4210526315789,-2.64999999999999));
#26999=CARTESIAN_POINT('Ctrl Pts',(-3.87986928011504,58.6184210526315,-3.87986928011504));
#27000=CARTESIAN_POINT('Ctrl Pts',(-2.65,58.8157894736842,-4.58993464005751));
#27001=CARTESIAN_POINT('Ctrl Pts',(-1.42013071988495,59.0131578947368,-5.29999999999999));
#27002=CARTESIAN_POINT('Ctrl Pts',(-6.49062803547473E-16,59.2105263157894,
-5.29999999999999));
#27003=CARTESIAN_POINT('Ctrl Pts',(1.42013071988495,59.4078947368421,-5.29999999999999));
#27004=CARTESIAN_POINT('Ctrl Pts',(2.64999999999999,59.6052631578947,-4.58993464005752));
#27005=CARTESIAN_POINT('Ctrl Pts',(3.87986928011504,59.8026315789473,-3.87986928011505));
#27006=CARTESIAN_POINT('Ctrl Pts',(4.58993464005751,60.,-2.65));
#27007=CARTESIAN_POINT('Ctrl Pts',(5.29999999999999,60.1973684210526,-1.42013071988495));
#27008=CARTESIAN_POINT('Ctrl Pts',(5.29999999999999,60.3947368421052,-9.73594205321184E-16));
#27009=CARTESIAN_POINT('Ctrl Pts',(5.29999999999999,60.5921052631579,1.42013071988495));
#27010=CARTESIAN_POINT('Ctrl Pts',(4.58993464005752,60.7894736842105,2.64999999999999));
#27011=CARTESIAN_POINT('Ctrl Pts',(3.87986928011505,60.9868421052632,3.87986928011504));
#27012=CARTESIAN_POINT('Ctrl Pts',(2.65,61.1842105263158,4.58993464005752));
#27013=CARTESIAN_POINT('Ctrl Pts',(1.42013071988495,61.3815789473684,5.29999999999998));
#27014=CARTESIAN_POINT('Ctrl Pts',(7.02579243712464E-28,61.5789473684211,
5.29999999999999));
#27015=CARTESIAN_POINT('Ctrl Pts',(-1.42013071988495,61.7763157894737,5.29999999999999));
#27016=CARTESIAN_POINT('Ctrl Pts',(-2.65,61.9736842105264,4.58993464005752));
#27017=CARTESIAN_POINT('Ctrl Pts',(-3.87986928011504,62.171052631579,3.87986928011505));
#27018=CARTESIAN_POINT('Ctrl Pts',(-4.58993464005751,62.3684210526316,2.65));
#27019=CARTESIAN_POINT('Ctrl Pts',(-5.29999999999999,62.5657894736842,1.42013071988495));
#27020=CARTESIAN_POINT('Ctrl Pts',(-5.29999999999999,62.7631578947368,3.24531401775109E-16));
#27021=CARTESIAN_POINT('Ctrl Pts',(-5.29999999999999,62.9605263157895,-1.42013071988495));
#27022=CARTESIAN_POINT('Ctrl Pts',(-4.58993464005751,63.1578947368421,-2.64999999999999));
#27023=CARTESIAN_POINT('Ctrl Pts',(-3.87986928011504,63.3552631578947,-3.87986928011504));
#27024=CARTESIAN_POINT('Ctrl Pts',(-2.65,63.5526315789474,-4.58993464005751));
#27025=CARTESIAN_POINT('Ctrl Pts',(-1.42013071988495,63.75,-5.29999999999999));
#27026=CARTESIAN_POINT('Ctrl Pts',(-6.49062803547422E-16,63.9473684210526,
-5.29999999999999));
#27027=CARTESIAN_POINT('Ctrl Pts',(1.42013071988495,64.1447368421053,-5.29999999999999));
#27028=CARTESIAN_POINT('Ctrl Pts',(2.64999999999999,64.3421052631579,-4.58993464005752));
#27029=CARTESIAN_POINT('Ctrl Pts',(3.87986928011504,64.5394736842105,-3.87986928011505));
#27030=CARTESIAN_POINT('Ctrl Pts',(4.58993464005751,64.7368421052632,-2.65));
#27031=CARTESIAN_POINT('Ctrl Pts',(5.29999999999999,64.9342105263157,-1.42013071988495));
#27032=CARTESIAN_POINT('Ctrl Pts',(5.29999999999999,65.1315789473684,-9.73594205320987E-16));
#27033=CARTESIAN_POINT('Ctrl Pts',(5.29999999999999,65.328947368421,1.42013071988495));
#27034=CARTESIAN_POINT('Ctrl Pts',(4.58993464005752,65.5263157894737,2.64999999999999));
#27035=CARTESIAN_POINT('Ctrl Pts',(3.87986928011505,65.7236842105264,3.87986928011504));
#27036=CARTESIAN_POINT('Ctrl Pts',(2.65,65.9210526315789,4.58993464005752));
#27037=CARTESIAN_POINT('Ctrl Pts',(1.42013071988495,66.1184210526315,5.29999999999999));
#27038=CARTESIAN_POINT('Ctrl Pts',(7.48801562377757E-28,66.3157894736842,
5.29999999999999));
#27039=CARTESIAN_POINT('Ctrl Pts',(-1.42013071988495,66.5131578947368,5.29999999999998));
#27040=CARTESIAN_POINT('Ctrl Pts',(-2.65,66.7105263157894,4.58993464005752));
#27041=CARTESIAN_POINT('Ctrl Pts',(-3.87986928011504,66.9078947368421,3.87986928011504));
#27042=CARTESIAN_POINT('Ctrl Pts',(-4.58993464005751,67.1052631578947,2.65));
#27043=CARTESIAN_POINT('Ctrl Pts',(-5.29999999999999,67.3026315789474,1.42013071988495));
#27044=CARTESIAN_POINT('Ctrl Pts',(-5.29999999999999,67.5,3.24531401774714E-16));
#27045=CARTESIAN_POINT('Ctrl Pts',(-5.29999999999999,67.6973684210526,-1.42013071988495));
#27046=CARTESIAN_POINT('Ctrl Pts',(-4.58993464005751,67.8947368421052,-2.64999999999999));
#27047=CARTESIAN_POINT('Ctrl Pts',(-3.87986928011504,68.0921052631578,-3.87986928011504));
#27048=CARTESIAN_POINT('Ctrl Pts',(-2.65,68.2894736842105,-4.58993464005751));
#27049=CARTESIAN_POINT('Ctrl Pts',(-1.42013071988495,68.4868421052632,-5.29999999999999));
#27050=CARTESIAN_POINT('Ctrl Pts',(-6.49062803547376E-16,68.6842105263158,
-5.29999999999999));
#27051=CARTESIAN_POINT('Ctrl Pts',(1.42013071988495,68.8815789473684,-5.29999999999999));
#27052=CARTESIAN_POINT('Ctrl Pts',(2.64999999999999,69.078947368421,-4.58993464005752));
#27053=CARTESIAN_POINT('Ctrl Pts',(3.87986928011504,69.2763157894736,-3.87986928011505));
#27054=CARTESIAN_POINT('Ctrl Pts',(4.58993464005751,69.4736842105263,-2.65));
#27055=CARTESIAN_POINT('Ctrl Pts',(5.29999999999999,69.6710526315789,-1.42013071988495));
#27056=CARTESIAN_POINT('Ctrl Pts',(5.29999999999999,69.8684210526316,-9.73594205320888E-16));
#27057=CARTESIAN_POINT('Ctrl Pts',(5.29999999999999,70.0657894736842,1.42013071988495));
#27058=CARTESIAN_POINT('Ctrl Pts',(4.58993464005752,70.2631578947369,2.64999999999999));
#27059=CARTESIAN_POINT('Ctrl Pts',(3.87986928011505,70.4605263157895,3.87986928011504));
#27060=CARTESIAN_POINT('Ctrl Pts',(2.65,70.6578947368421,4.58993464005752));
#27061=CARTESIAN_POINT('Ctrl Pts',(1.42013071988495,70.8552631578947,5.29999999999998));
#27062=CARTESIAN_POINT('Ctrl Pts',(7.96564624998561E-28,71.0526315789473,
5.29999999999999));
#27063=CARTESIAN_POINT('Ctrl Pts',(-1.42013071988495,71.2499999999999,5.29999999999999));
#27064=CARTESIAN_POINT('Ctrl Pts',(-2.65,71.4473684210526,4.58993464005751));
#27065=CARTESIAN_POINT('Ctrl Pts',(-3.87986928011504,71.6447368421053,3.87986928011504));
#27066=CARTESIAN_POINT('Ctrl Pts',(-4.58993464005751,71.8421052631579,2.65));
#27067=CARTESIAN_POINT('Ctrl Pts',(-5.29999999999999,72.0394736842105,1.42013071988495));
#27068=CARTESIAN_POINT('Ctrl Pts',(-5.29999999999999,72.2368421052632,3.24531401775306E-16));
#27069=CARTESIAN_POINT('Ctrl Pts',(-5.29999999999999,72.4342105263157,-1.42013071988495));
#27070=CARTESIAN_POINT('Ctrl Pts',(-4.58993464005751,72.6315789473684,-2.64999999999999));
#27071=CARTESIAN_POINT('Ctrl Pts',(-3.87986928011504,72.828947368421,-3.87986928011504));
#27072=CARTESIAN_POINT('Ctrl Pts',(-2.65,73.0263157894737,-4.58993464005751));
#27073=CARTESIAN_POINT('Ctrl Pts',(-1.42013071988495,73.2236842105263,-5.29999999999999));
#27074=CARTESIAN_POINT('Ctrl Pts',(-6.4906280354732E-16,73.421052631579,
-5.29999999999999));
#27075=CARTESIAN_POINT('Ctrl Pts',(1.42013071988495,73.6184210526315,-5.29999999999999));
#27076=CARTESIAN_POINT('Ctrl Pts',(2.64999999999999,73.8157894736842,-4.58993464005751));
#27077=CARTESIAN_POINT('Ctrl Pts',(3.87986928011504,74.0131578947368,-3.87986928011505));
#27078=CARTESIAN_POINT('Ctrl Pts',(4.58993464005751,74.2105263157895,-2.65));
#27079=CARTESIAN_POINT('Ctrl Pts',(5.29999999999999,74.4078947368421,-1.42013071988495));
#27080=CARTESIAN_POINT('Ctrl Pts',(5.29999999999999,74.6052631578947,-9.73594205321085E-16));
#27081=CARTESIAN_POINT('Ctrl Pts',(5.29999999999999,74.8026315789473,1.42013071988495));
#27082=CARTESIAN_POINT('Ctrl Pts',(4.58993464005752,75.,2.64999999999999));
#27083=CARTESIAN_POINT('Ctrl Pts',(3.87986928011505,75.1973684210526,3.87986928011504));
#27084=CARTESIAN_POINT('Ctrl Pts',(2.65,75.3947368421052,4.58993464005751));
#27085=CARTESIAN_POINT('Ctrl Pts',(1.42013071988495,75.5921052631578,5.29999999999998));
#27086=CARTESIAN_POINT('Ctrl Pts',(8.68979590907521E-28,75.7894736842105,
5.29999999999999));
#27087=CARTESIAN_POINT('Ctrl Pts',(-1.42013071988495,75.9868421052631,5.29999999999999));
#27088=CARTESIAN_POINT('Ctrl Pts',(-2.65,76.1842105263158,4.58993464005751));
#27089=CARTESIAN_POINT('Ctrl Pts',(-3.87986928011504,76.3815789473684,3.87986928011504));
#27090=CARTESIAN_POINT('Ctrl Pts',(-4.58993464005751,76.5789473684211,2.65));
#27091=CARTESIAN_POINT('Ctrl Pts',(-5.29999999999999,76.7763157894737,1.42013071988495));
#27092=CARTESIAN_POINT('Ctrl Pts',(-5.29999999999999,76.9736842105263,3.24531401774615E-16));
#27093=CARTESIAN_POINT('Ctrl Pts',(-5.29999999999999,77.1710526315789,-1.42013071988495));
#27094=CARTESIAN_POINT('Ctrl Pts',(-4.58993464005751,77.3684210526315,-2.64999999999999));
#27095=CARTESIAN_POINT('Ctrl Pts',(-3.87986928011504,77.5657894736842,-3.87986928011504));
#27096=CARTESIAN_POINT('Ctrl Pts',(-2.65,77.7631578947368,-4.58993464005751));
#27097=CARTESIAN_POINT('Ctrl Pts',(-1.42013071988495,77.9605263157895,-5.29999999999999));
#27098=CARTESIAN_POINT('Ctrl Pts',(-6.49062803547265E-16,78.1578947368421,
-5.29999999999999));
#27099=CARTESIAN_POINT('Ctrl Pts',(1.42013071988495,78.3552631578948,-5.29999999999999));
#27100=CARTESIAN_POINT('Ctrl Pts',(2.64999999999999,78.5526315789474,-4.58993464005751));
#27101=CARTESIAN_POINT('Ctrl Pts',(3.87986928011504,78.7499999999999,-3.87986928011505));
#27102=CARTESIAN_POINT('Ctrl Pts',(4.58993464005751,78.9473684210526,-2.65));
#27103=CARTESIAN_POINT('Ctrl Pts',(5.29999999999999,79.1447368421052,-1.42013071988495));
#27104=CARTESIAN_POINT('Ctrl Pts',(5.29999999999999,79.3421052631579,-9.73594205320987E-16));
#27105=CARTESIAN_POINT('Ctrl Pts',(5.29999999999999,79.5394736842105,1.42013071988495));
#27106=CARTESIAN_POINT('Ctrl Pts',(4.58993464005752,79.7368421052632,2.64999999999999));
#27107=CARTESIAN_POINT('Ctrl Pts',(3.87986928011505,79.9342105263158,3.87986928011504));
#27108=CARTESIAN_POINT('Ctrl Pts',(2.65,80.1315789473684,4.58993464005751));
#27109=CARTESIAN_POINT('Ctrl Pts',(1.42013071988495,80.328947368421,5.29999999999999));
#27110=CARTESIAN_POINT('Ctrl Pts',(9.15201909572814E-28,80.5263157894736,
5.3));
#27111=CARTESIAN_POINT('Ctrl Pts',(-1.42013071988495,80.7236842105263,5.29999999999998));
#27112=CARTESIAN_POINT('Ctrl Pts',(-2.65,80.9210526315789,4.58993464005751));
#27113=CARTESIAN_POINT('Ctrl Pts',(-3.87986928011504,81.1184210526315,3.87986928011504));
#27114=CARTESIAN_POINT('Ctrl Pts',(-4.58993464005751,81.3157894736842,2.64999999999999));
#27115=CARTESIAN_POINT('Ctrl Pts',(-5.29999999999999,81.5131578947368,1.42013071988495));
#27116=CARTESIAN_POINT('Ctrl Pts',(-5.29999999999999,81.7105263157895,3.24531401775207E-16));
#27117=CARTESIAN_POINT('Ctrl Pts',(-5.29999999999999,81.9078947368421,-1.42013071988495));
#27118=CARTESIAN_POINT('Ctrl Pts',(-4.58993464005751,82.1052631578947,-2.64999999999999));
#27119=CARTESIAN_POINT('Ctrl Pts',(-3.87986928011504,82.3026315789473,-3.87986928011504));
#27120=CARTESIAN_POINT('Ctrl Pts',(-2.65,82.5,-4.58993464005751));
#27121=CARTESIAN_POINT('Ctrl Pts',(-1.42013071988495,82.6973684210527,-5.29999999999999));
#27122=CARTESIAN_POINT('Ctrl Pts',(-6.49062803547219E-16,82.8947368421053,
-5.29999999999999));
#27123=CARTESIAN_POINT('Ctrl Pts',(1.42013071988495,83.0921052631579,-5.29999999999999));
#27124=CARTESIAN_POINT('Ctrl Pts',(2.64999999999999,83.2894736842105,-4.58993464005751));
#27125=CARTESIAN_POINT('Ctrl Pts',(3.87986928011504,83.4868421052631,-3.87986928011505));
#27126=CARTESIAN_POINT('Ctrl Pts',(4.58993464005751,83.6842105263158,-2.65));
#27127=CARTESIAN_POINT('Ctrl Pts',(5.29999999999999,83.8815789473684,-1.42013071988495));
#27128=CARTESIAN_POINT('Ctrl Pts',(5.29999999999999,84.078947368421,-9.73594205321184E-16));
#27129=CARTESIAN_POINT('Ctrl Pts',(5.29999999999999,84.2763157894736,1.42013071988495));
#27130=CARTESIAN_POINT('Ctrl Pts',(4.58993464005752,84.4736842105263,2.64999999999999));
#27131=CARTESIAN_POINT('Ctrl Pts',(3.87986928011505,84.6710526315789,3.87986928011504));
#27132=CARTESIAN_POINT('Ctrl Pts',(2.65,84.8684210526316,4.58993464005751));
#27133=CARTESIAN_POINT('Ctrl Pts',(1.42013071988495,85.0657894736842,5.29999999999998));
#27134=CARTESIAN_POINT('Ctrl Pts',(9.61424228238108E-28,85.2631578947368,
5.3));
#27135=CARTESIAN_POINT('Ctrl Pts',(-1.42013071988495,85.4605263157894,5.29999999999999));
#27136=CARTESIAN_POINT('Ctrl Pts',(-2.65,85.6578947368421,4.58993464005751));
#27137=CARTESIAN_POINT('Ctrl Pts',(-3.87986928011504,85.8552631578947,3.87986928011504));
#27138=CARTESIAN_POINT('Ctrl Pts',(-4.58993464005751,86.0526315789474,2.65));
#27139=CARTESIAN_POINT('Ctrl Pts',(-5.29999999999999,86.25,1.42013071988495));
#27140=CARTESIAN_POINT('Ctrl Pts',(-5.29999999999999,86.4473684210526,3.24531401775207E-16));
#27141=CARTESIAN_POINT('Ctrl Pts',(-5.29999999999999,86.6447368421052,-1.42013071988495));
#27142=CARTESIAN_POINT('Ctrl Pts',(-4.58993464005751,86.8421052631579,-2.64999999999999));
#27143=CARTESIAN_POINT('Ctrl Pts',(-3.87986928011504,87.0394736842105,-3.87986928011504));
#27144=CARTESIAN_POINT('Ctrl Pts',(-2.65,87.2368421052631,-4.58993464005751));
#27145=CARTESIAN_POINT('Ctrl Pts',(-1.42013071988495,87.4342105263158,-5.29999999999999));
#27146=CARTESIAN_POINT('Ctrl Pts',(-6.49062803547173E-16,87.6315789473684,
-5.29999999999999));
#27147=CARTESIAN_POINT('Ctrl Pts',(1.42013071988495,87.828947368421,-5.29999999999999));
#27148=CARTESIAN_POINT('Ctrl Pts',(2.64999999999999,88.0263157894737,-4.58993464005751));
#27149=CARTESIAN_POINT('Ctrl Pts',(3.87986928011504,88.2236842105263,-3.87986928011505));
#27150=CARTESIAN_POINT('Ctrl Pts',(4.58993464005751,88.4210526315789,-2.65));
#27151=CARTESIAN_POINT('Ctrl Pts',(5.29999999999999,88.6184210526316,-1.42013071988495));
#27152=CARTESIAN_POINT('Ctrl Pts',(5.29999999999999,88.8157894736842,-9.73594205321085E-16));
#27153=CARTESIAN_POINT('Ctrl Pts',(5.29999999999999,89.0131578947368,1.42013071988495));
#27154=CARTESIAN_POINT('Ctrl Pts',(4.58993464005752,89.2105263157895,2.64999999999999));
#27155=CARTESIAN_POINT('Ctrl Pts',(3.87986928011505,89.4078947368421,3.87986928011504));
#27156=CARTESIAN_POINT('Ctrl Pts',(2.65,89.6052631578947,4.58993464005751));
#27157=CARTESIAN_POINT('Ctrl Pts',(1.42013071988495,89.8026315789473,5.29999999999999));
#27158=CARTESIAN_POINT('Ctrl Pts',(1.01689101063646E-27,89.9999999999999,
5.3));
#27159=CARTESIAN_POINT('Ctrl Pts',(2.77333911991762E-29,0.,5.29999999999999));
#27160=CARTESIAN_POINT('Ctrl Pts',(-1.42013071988495,0.197368421052638,
5.29999999999998));
#27161=CARTESIAN_POINT('Ctrl Pts',(-2.65,0.394736842105281,4.58993464005751));
#27162=CARTESIAN_POINT('Ctrl Pts',(-3.87986928011504,0.592105263157915,
3.87986928011505));
#27163=CARTESIAN_POINT('Ctrl Pts',(-4.58993464005751,0.789473684210562,
2.65));
#27164=CARTESIAN_POINT('Ctrl Pts',(-5.29999999999999,0.986842105263191,
1.42013071988495));
#27165=CARTESIAN_POINT('Ctrl Pts',(-5.29999999999999,1.18421052631579,3.24531401774024E-16));
#27166=CARTESIAN_POINT('Ctrl Pts',(-5.29999999999999,1.38157894736841,-1.42013071988495));
#27167=CARTESIAN_POINT('Ctrl Pts',(-4.58993464005751,1.57894736842107,-2.64999999999999));
#27168=CARTESIAN_POINT('Ctrl Pts',(-3.87986928011504,1.77631578947369,-3.87986928011504));
#27169=CARTESIAN_POINT('Ctrl Pts',(-2.65,1.97368421052629,-4.58993464005751));
#27170=CARTESIAN_POINT('Ctrl Pts',(-1.42013071988495,2.17105263157891,-5.29999999999999));
#27171=CARTESIAN_POINT('Ctrl Pts',(-6.49062803548097E-16,2.36842105263158,
-5.29999999999999));
#27172=CARTESIAN_POINT('Ctrl Pts',(1.42013071988495,2.56578947368418,-5.29999999999999));
#27173=CARTESIAN_POINT('Ctrl Pts',(2.64999999999999,2.7631578947368,-4.58993464005751));
#27174=CARTESIAN_POINT('Ctrl Pts',(3.87986928011504,2.96052631578946,-3.87986928011505));
#27175=CARTESIAN_POINT('Ctrl Pts',(4.58993464005751,3.15789473684208,-2.65));
#27176=CARTESIAN_POINT('Ctrl Pts',(5.29999999999999,3.35526315789473,-1.42013071988495));
#27177=CARTESIAN_POINT('Ctrl Pts',(5.29999999999999,3.55263157894736,-9.73594205321085E-16));
#27178=CARTESIAN_POINT('Ctrl Pts',(5.29999999999999,3.75000000000001,1.42013071988494));
#27179=CARTESIAN_POINT('Ctrl Pts',(4.58993464005752,3.94736842105264,2.64999999999999));
#27180=CARTESIAN_POINT('Ctrl Pts',(3.87986928011505,4.14473684210529,3.87986928011504));
#27181=CARTESIAN_POINT('Ctrl Pts',(2.65,4.34210526315792,4.58993464005751));
#27182=CARTESIAN_POINT('Ctrl Pts',(1.42013071988495,4.53947368421056,5.29999999999998));
#27183=CARTESIAN_POINT('Ctrl Pts',(8.32001735975286E-29,4.73684210526315,
5.29999999999999));
#27184=CARTESIAN_POINT('Ctrl Pts',(-1.42013071988495,4.93421052631578,5.29999999999999));
#27185=CARTESIAN_POINT('Ctrl Pts',(-2.65,5.13157894736843,4.58993464005751));
#27186=CARTESIAN_POINT('Ctrl Pts',(-3.87986928011504,5.32894736842106,3.87986928011505));
#27187=CARTESIAN_POINT('Ctrl Pts',(-4.58993464005751,5.52631578947371,2.65));
#27188=CARTESIAN_POINT('Ctrl Pts',(-5.29999999999999,5.72368421052634,1.42013071988495));
#27189=CARTESIAN_POINT('Ctrl Pts',(-5.29999999999999,5.92105263157894,3.24531401774024E-16));
#27190=CARTESIAN_POINT('Ctrl Pts',(-5.29999999999999,6.11842105263156,-1.42013071988495));
#27191=CARTESIAN_POINT('Ctrl Pts',(-4.58993464005751,6.31578947368422,-2.64999999999999));
#27192=CARTESIAN_POINT('Ctrl Pts',(-3.87986928011504,6.51315789473683,-3.87986928011504));
#27193=CARTESIAN_POINT('Ctrl Pts',(-2.65,6.71052631578944,-4.58993464005751));
#27194=CARTESIAN_POINT('Ctrl Pts',(-1.42013071988495,6.90789473684211,-5.29999999999999));
#27195=CARTESIAN_POINT('Ctrl Pts',(-6.49062803548043E-16,7.10526315789473,
-5.29999999999999));
#27196=CARTESIAN_POINT('Ctrl Pts',(1.42013071988495,7.30263157894733,-5.29999999999999));
#27197=CARTESIAN_POINT('Ctrl Pts',(2.64999999999999,7.50000000000001,-4.58993464005751));
#27198=CARTESIAN_POINT('Ctrl Pts',(3.87986928011504,7.69736842105261,-3.87986928011505));
#27199=CARTESIAN_POINT('Ctrl Pts',(4.58993464005751,7.89473684210523,-2.65));
#27200=CARTESIAN_POINT('Ctrl Pts',(5.29999999999999,8.09210526315788,-1.42013071988495));
#27201=CARTESIAN_POINT('Ctrl Pts',(5.29999999999999,8.28947368421051,-9.73594205321085E-16));
#27202=CARTESIAN_POINT('Ctrl Pts',(5.29999999999999,8.48684210526316,1.42013071988495));
#27203=CARTESIAN_POINT('Ctrl Pts',(4.58993464005752,8.68421052631579,2.64999999999999));
#27204=CARTESIAN_POINT('Ctrl Pts',(3.87986928011505,8.88157894736843,3.87986928011504));
#27205=CARTESIAN_POINT('Ctrl Pts',(2.65,9.07894736842108,4.58993464005751));
#27206=CARTESIAN_POINT('Ctrl Pts',(1.42013071988495,9.27631578947371,5.29999999999999));
#27207=CARTESIAN_POINT('Ctrl Pts',(1.35585468084861E-28,9.47368421052636,
5.3));
#27208=CARTESIAN_POINT('Ctrl Pts',(-1.42013071988495,9.67105263157899,5.29999999999998));
#27209=CARTESIAN_POINT('Ctrl Pts',(-2.65,9.86842105263158,4.58993464005751));
#27210=CARTESIAN_POINT('Ctrl Pts',(-3.87986928011504,10.0657894736842,3.87986928011504));
#27211=CARTESIAN_POINT('Ctrl Pts',(-4.58993464005751,10.2631578947369,2.65));
#27212=CARTESIAN_POINT('Ctrl Pts',(-5.29999999999999,10.4605263157895,1.42013071988495));
#27213=CARTESIAN_POINT('Ctrl Pts',(-5.29999999999999,10.6578947368421,3.24531401772841E-16));
#27214=CARTESIAN_POINT('Ctrl Pts',(-5.29999999999999,10.8552631578948,-1.42013071988495));
#27215=CARTESIAN_POINT('Ctrl Pts',(-4.58993464005751,11.0526315789474,-2.64999999999999));
#27216=CARTESIAN_POINT('Ctrl Pts',(-3.87986928011504,11.25,-3.87986928011504));
#27217=CARTESIAN_POINT('Ctrl Pts',(-2.65,11.4473684210526,-4.58993464005751));
#27218=CARTESIAN_POINT('Ctrl Pts',(-1.42013071988495,11.6447368421052,-5.29999999999999));
#27219=CARTESIAN_POINT('Ctrl Pts',(-6.49062803547995E-16,11.8421052631579,
-5.29999999999999));
#27220=CARTESIAN_POINT('Ctrl Pts',(1.42013071988495,12.0394736842105,-5.29999999999999));
#27221=CARTESIAN_POINT('Ctrl Pts',(2.64999999999999,12.2368421052632,-4.58993464005751));
#27222=CARTESIAN_POINT('Ctrl Pts',(3.87986928011504,12.4342105263158,-3.87986928011505));
#27223=CARTESIAN_POINT('Ctrl Pts',(4.58993464005751,12.6315789473684,-2.65));
#27224=CARTESIAN_POINT('Ctrl Pts',(5.29999999999999,12.828947368421,-1.42013071988495));
#27225=CARTESIAN_POINT('Ctrl Pts',(5.29999999999999,13.0263157894737,-9.73594205322072E-16));
#27226=CARTESIAN_POINT('Ctrl Pts',(5.29999999999999,13.2236842105263,1.42013071988495));
#27227=CARTESIAN_POINT('Ctrl Pts',(4.58993464005752,13.4210526315789,2.64999999999999));
#27228=CARTESIAN_POINT('Ctrl Pts',(3.87986928011505,13.6184210526316,3.87986928011504));
#27229=CARTESIAN_POINT('Ctrl Pts',(2.65,13.8157894736842,4.58993464005751));
#27230=CARTESIAN_POINT('Ctrl Pts',(1.42013071988495,14.0131578947369,5.29999999999998));
#27231=CARTESIAN_POINT('Ctrl Pts',(1.84889274661175E-28,14.2105263157895,
5.3));
#27232=CARTESIAN_POINT('Ctrl Pts',(-1.42013071988495,14.4078947368421,5.29999999999999));
#27233=CARTESIAN_POINT('Ctrl Pts',(-2.65,14.6052631578947,4.58993464005751));
#27234=CARTESIAN_POINT('Ctrl Pts',(-3.87986928011504,14.8026315789474,3.87986928011504));
#27235=CARTESIAN_POINT('Ctrl Pts',(-4.58993464005751,15.,2.65));
#27236=CARTESIAN_POINT('Ctrl Pts',(-5.29999999999999,15.1973684210526,1.42013071988495));
#27237=CARTESIAN_POINT('Ctrl Pts',(-5.29999999999999,15.3947368421052,3.24531401774024E-16));
#27238=CARTESIAN_POINT('Ctrl Pts',(-5.29999999999999,15.5921052631579,-1.42013071988495));
#27239=CARTESIAN_POINT('Ctrl Pts',(-4.58993464005751,15.7894736842105,-2.64999999999999));
#27240=CARTESIAN_POINT('Ctrl Pts',(-3.87986928011504,15.9868421052631,-3.87986928011504));
#27241=CARTESIAN_POINT('Ctrl Pts',(-2.65,16.1842105263157,-4.58993464005751));
#27242=CARTESIAN_POINT('Ctrl Pts',(-1.42013071988495,16.3815789473684,-5.29999999999999));
#27243=CARTESIAN_POINT('Ctrl Pts',(-6.49062803547949E-16,16.578947368421,
-5.29999999999999));
#27244=CARTESIAN_POINT('Ctrl Pts',(1.42013071988495,16.7763157894737,-5.29999999999999));
#27245=CARTESIAN_POINT('Ctrl Pts',(2.64999999999999,16.9736842105263,-4.58993464005751));
#27246=CARTESIAN_POINT('Ctrl Pts',(3.87986928011504,17.171052631579,-3.87986928011505));
#27247=CARTESIAN_POINT('Ctrl Pts',(4.58993464005751,17.3684210526316,-2.65));
#27248=CARTESIAN_POINT('Ctrl Pts',(5.29999999999999,17.5657894736842,-1.42013071988495));
#27249=CARTESIAN_POINT('Ctrl Pts',(5.29999999999999,17.7631578947368,-9.73594205322269E-16));
#27250=CARTESIAN_POINT('Ctrl Pts',(5.29999999999999,17.9605263157895,1.42013071988494));
#27251=CARTESIAN_POINT('Ctrl Pts',(4.58993464005752,18.1578947368421,2.64999999999999));
#27252=CARTESIAN_POINT('Ctrl Pts',(3.87986928011505,18.3552631578947,3.87986928011504));
#27253=CARTESIAN_POINT('Ctrl Pts',(2.65,18.5526315789474,4.58993464005751));
#27254=CARTESIAN_POINT('Ctrl Pts',(1.42013071988495,18.75,5.29999999999998));
#27255=CARTESIAN_POINT('Ctrl Pts',(2.31111593326468E-28,18.9473684210527,
5.3));
#27256=CARTESIAN_POINT('Ctrl Pts',(-1.42013071988495,19.1447368421053,5.29999999999999));
#27257=CARTESIAN_POINT('Ctrl Pts',(-2.65,19.3421052631579,4.58993464005751));
#27258=CARTESIAN_POINT('Ctrl Pts',(-3.87986928011504,19.5394736842105,3.87986928011504));
#27259=CARTESIAN_POINT('Ctrl Pts',(-4.58993464005751,19.7368421052632,2.65));
#27260=CARTESIAN_POINT('Ctrl Pts',(-5.29999999999999,19.9342105263158,1.42013071988495));
#27261=CARTESIAN_POINT('Ctrl Pts',(-5.29999999999999,20.1315789473684,3.24531401774221E-16));
#27262=CARTESIAN_POINT('Ctrl Pts',(-5.29999999999999,20.328947368421,-1.42013071988495));
#27263=CARTESIAN_POINT('Ctrl Pts',(-4.58993464005751,20.5263157894737,-2.64999999999999));
#27264=CARTESIAN_POINT('Ctrl Pts',(-3.87986928011504,20.7236842105263,-3.87986928011504));
#27265=CARTESIAN_POINT('Ctrl Pts',(-2.65,20.921052631579,-4.58993464005751));
#27266=CARTESIAN_POINT('Ctrl Pts',(-1.42013071988495,21.1184210526315,-5.29999999999999));
#27267=CARTESIAN_POINT('Ctrl Pts',(-6.49062803547894E-16,21.3157894736842,
-5.29999999999999));
#27268=CARTESIAN_POINT('Ctrl Pts',(1.42013071988495,21.5131578947368,-5.29999999999999));
#27269=CARTESIAN_POINT('Ctrl Pts',(2.64999999999999,21.7105263157895,-4.58993464005751));
#27270=CARTESIAN_POINT('Ctrl Pts',(3.87986928011504,21.9078947368421,-3.87986928011505));
#27271=CARTESIAN_POINT('Ctrl Pts',(4.58993464005751,22.1052631578947,-2.65));
#27272=CARTESIAN_POINT('Ctrl Pts',(5.29999999999999,22.3026315789474,-1.42013071988495));
#27273=CARTESIAN_POINT('Ctrl Pts',(5.29999999999999,22.5,-9.73594205320888E-16));
#27274=CARTESIAN_POINT('Ctrl Pts',(5.29999999999999,22.6973684210527,1.42013071988495));
#27275=CARTESIAN_POINT('Ctrl Pts',(4.58993464005752,22.8947368421052,2.64999999999999));
#27276=CARTESIAN_POINT('Ctrl Pts',(3.87986928011505,23.0921052631579,3.87986928011504));
#27277=CARTESIAN_POINT('Ctrl Pts',(2.65,23.2894736842105,4.58993464005751));
#27278=CARTESIAN_POINT('Ctrl Pts',(1.42013071988495,23.4868421052631,5.29999999999999));
#27279=CARTESIAN_POINT('Ctrl Pts',(2.95822839457879E-28,23.6842105263158,
5.3));
#27280=CARTESIAN_POINT('Ctrl Pts',(-1.42013071988495,23.8815789473684,5.29999999999998));
#27281=CARTESIAN_POINT('Ctrl Pts',(-2.65,24.0789473684211,4.58993464005751));
#27282=CARTESIAN_POINT('Ctrl Pts',(-3.87986928011504,24.2763157894737,3.87986928011504));
#27283=CARTESIAN_POINT('Ctrl Pts',(-4.58993464005751,24.4736842105263,2.65));
#27284=CARTESIAN_POINT('Ctrl Pts',(-5.29999999999999,24.671052631579,1.42013071988495));
#27285=CARTESIAN_POINT('Ctrl Pts',(-5.29999999999999,24.8684210526316,3.24531401774024E-16));
#27286=CARTESIAN_POINT('Ctrl Pts',(-5.29999999999999,25.0657894736842,-1.42013071988495));
#27287=CARTESIAN_POINT('Ctrl Pts',(-4.58993464005751,25.2631578947368,-2.64999999999999));
#27288=CARTESIAN_POINT('Ctrl Pts',(-3.87986928011504,25.4605263157895,-3.87986928011504));
#27289=CARTESIAN_POINT('Ctrl Pts',(-2.65,25.6578947368421,-4.58993464005751));
#27290=CARTESIAN_POINT('Ctrl Pts',(-1.42013071988495,25.8552631578947,-5.29999999999999));
#27291=CARTESIAN_POINT('Ctrl Pts',(-6.49062803547834E-16,26.0526315789473,
-5.29999999999999));
#27292=CARTESIAN_POINT('Ctrl Pts',(1.42013071988495,26.25,-5.29999999999999));
#27293=CARTESIAN_POINT('Ctrl Pts',(2.64999999999999,26.4473684210526,-4.58993464005752));
#27294=CARTESIAN_POINT('Ctrl Pts',(3.87986928011504,26.6447368421052,-3.87986928011505));
#27295=CARTESIAN_POINT('Ctrl Pts',(4.58993464005751,26.8421052631579,-2.65));
#27296=CARTESIAN_POINT('Ctrl Pts',(5.29999999999999,27.0394736842105,-1.42013071988495));
#27297=CARTESIAN_POINT('Ctrl Pts',(5.29999999999999,27.2368421052632,-9.73594205320888E-16));
#27298=CARTESIAN_POINT('Ctrl Pts',(5.29999999999999,27.4342105263158,1.42013071988495));
#27299=CARTESIAN_POINT('Ctrl Pts',(4.58993464005752,27.6315789473685,2.64999999999999));
#27300=CARTESIAN_POINT('Ctrl Pts',(3.87986928011505,27.8289473684211,3.87986928011504));
#27301=CARTESIAN_POINT('Ctrl Pts',(2.65,28.0263157894737,4.58993464005751));
#27302=CARTESIAN_POINT('Ctrl Pts',(1.42013071988495,28.2236842105264,5.29999999999998));
#27303=CARTESIAN_POINT('Ctrl Pts',(3.42045158123173E-28,28.421052631579,
5.3));
#27304=CARTESIAN_POINT('Ctrl Pts',(-1.42013071988495,28.6184210526316,5.29999999999999));
#27305=CARTESIAN_POINT('Ctrl Pts',(-2.65,28.8157894736842,4.58993464005751));
#27306=CARTESIAN_POINT('Ctrl Pts',(-3.87986928011504,29.0131578947368,3.87986928011504));
#27307=CARTESIAN_POINT('Ctrl Pts',(-4.58993464005751,29.2105263157895,2.65));
#27308=CARTESIAN_POINT('Ctrl Pts',(-5.29999999999999,29.4078947368421,1.42013071988495));
#27309=CARTESIAN_POINT('Ctrl Pts',(-5.29999999999999,29.6052631578947,3.24531401774024E-16));
#27310=CARTESIAN_POINT('Ctrl Pts',(-5.29999999999999,29.8026315789473,-1.42013071988495));
#27311=CARTESIAN_POINT('Ctrl Pts',(-4.58993464005751,30.,-2.64999999999999));
#27312=CARTESIAN_POINT('Ctrl Pts',(-3.87986928011504,30.1973684210526,-3.87986928011504));
#27313=CARTESIAN_POINT('Ctrl Pts',(-2.65,30.3947368421053,-4.58993464005751));
#27314=CARTESIAN_POINT('Ctrl Pts',(-1.42013071988495,30.5921052631579,-5.29999999999999));
#27315=CARTESIAN_POINT('Ctrl Pts',(-6.49062803547783E-16,30.7894736842105,
-5.29999999999999));
#27316=CARTESIAN_POINT('Ctrl Pts',(1.42013071988495,30.9868421052631,-5.29999999999999));
#27317=CARTESIAN_POINT('Ctrl Pts',(2.64999999999999,31.1842105263158,-4.58993464005752));
#27318=CARTESIAN_POINT('Ctrl Pts',(3.87986928011504,31.3815789473684,-3.87986928011505));
#27319=CARTESIAN_POINT('Ctrl Pts',(4.58993464005751,31.578947368421,-2.65));
#27320=CARTESIAN_POINT('Ctrl Pts',(5.29999999999999,31.7763157894737,-1.42013071988495));
#27321=CARTESIAN_POINT('Ctrl Pts',(5.29999999999999,31.9736842105263,-9.73594205321085E-16));
#27322=CARTESIAN_POINT('Ctrl Pts',(5.29999999999999,32.1710526315789,1.42013071988495));
#27323=CARTESIAN_POINT('Ctrl Pts',(4.58993464005752,32.3684210526316,2.64999999999999));
#27324=CARTESIAN_POINT('Ctrl Pts',(3.87986928011505,32.5657894736842,3.87986928011504));
#27325=CARTESIAN_POINT('Ctrl Pts',(2.65,32.7631578947368,4.58993464005751));
#27326=CARTESIAN_POINT('Ctrl Pts',(1.42013071988495,32.9605263157895,5.29999999999999));
#27327=CARTESIAN_POINT('Ctrl Pts',(3.88267476788467E-28,33.1578947368421,
5.3));
#27328=CARTESIAN_POINT('Ctrl Pts',(-1.42013071988495,33.3552631578948,5.29999999999998));
#27329=CARTESIAN_POINT('Ctrl Pts',(-2.65,33.5526315789474,4.58993464005751));
#27330=CARTESIAN_POINT('Ctrl Pts',(-3.87986928011504,33.75,3.87986928011505));
#27331=CARTESIAN_POINT('Ctrl Pts',(-4.58993464005751,33.9473684210526,2.65));
#27332=CARTESIAN_POINT('Ctrl Pts',(-5.29999999999999,34.1447368421052,1.42013071988495));
#27333=CARTESIAN_POINT('Ctrl Pts',(-5.29999999999999,34.3421052631579,3.24531401774024E-16));
#27334=CARTESIAN_POINT('Ctrl Pts',(-5.29999999999999,34.5394736842105,-1.42013071988495));
#27335=CARTESIAN_POINT('Ctrl Pts',(-4.58993464005751,34.7368421052631,-2.65));
#27336=CARTESIAN_POINT('Ctrl Pts',(-3.87986928011504,34.9342105263158,-3.87986928011504));
#27337=CARTESIAN_POINT('Ctrl Pts',(-2.65,35.1315789473684,-4.58993464005751));
#27338=CARTESIAN_POINT('Ctrl Pts',(-1.42013071988495,35.328947368421,-5.29999999999999));
#27339=CARTESIAN_POINT('Ctrl Pts',(-6.49062803547736E-16,35.5263157894737,
-5.29999999999999));
#27340=CARTESIAN_POINT('Ctrl Pts',(1.42013071988495,35.7236842105263,-5.29999999999999));
#27341=CARTESIAN_POINT('Ctrl Pts',(2.64999999999999,35.9210526315789,-4.58993464005752));
#27342=CARTESIAN_POINT('Ctrl Pts',(3.87986928011504,36.1184210526315,-3.87986928011505));
#27343=CARTESIAN_POINT('Ctrl Pts',(4.58993464005751,36.3157894736842,-2.65));
#27344=CARTESIAN_POINT('Ctrl Pts',(5.29999999999999,36.5131578947368,-1.42013071988495));
#27345=CARTESIAN_POINT('Ctrl Pts',(5.29999999999999,36.7105263157895,-9.73594205322072E-16));
#27346=CARTESIAN_POINT('Ctrl Pts',(5.29999999999999,36.9078947368421,1.42013071988495));
#27347=CARTESIAN_POINT('Ctrl Pts',(4.58993464005752,37.1052631578948,2.64999999999999));
#27348=CARTESIAN_POINT('Ctrl Pts',(3.87986928011505,37.3026315789473,3.87986928011504));
#27349=CARTESIAN_POINT('Ctrl Pts',(2.65,37.5,4.58993464005751));
#27350=CARTESIAN_POINT('Ctrl Pts',(1.42013071988495,37.6973684210526,5.29999999999998));
#27351=CARTESIAN_POINT('Ctrl Pts',(4.42193515231309E-28,37.8947368421053,
5.29999999999999));
#27352=CARTESIAN_POINT('Ctrl Pts',(-1.42013071988495,38.0921052631579,5.29999999999999));
#27353=CARTESIAN_POINT('Ctrl Pts',(-2.65,38.2894736842105,4.58993464005752));
#27354=CARTESIAN_POINT('Ctrl Pts',(-3.87986928011504,38.4868421052632,3.87986928011504));
#27355=CARTESIAN_POINT('Ctrl Pts',(-4.58993464005751,38.6842105263158,2.65));
#27356=CARTESIAN_POINT('Ctrl Pts',(-5.29999999999999,38.8815789473684,1.42013071988495));
#27357=CARTESIAN_POINT('Ctrl Pts',(-5.29999999999999,39.078947368421,3.24531401774024E-16));
#27358=CARTESIAN_POINT('Ctrl Pts',(-5.29999999999999,39.2763157894737,-1.42013071988495));
#27359=CARTESIAN_POINT('Ctrl Pts',(-4.58993464005751,39.4736842105263,-2.64999999999999));
#27360=CARTESIAN_POINT('Ctrl Pts',(-3.87986928011504,39.6710526315789,-3.87986928011504));
#27361=CARTESIAN_POINT('Ctrl Pts',(-2.65,39.8684210526316,-4.58993464005751));
#27362=CARTESIAN_POINT('Ctrl Pts',(-1.42013071988495,40.0657894736842,-5.29999999999999));
#27363=CARTESIAN_POINT('Ctrl Pts',(-6.49062803547683E-16,40.2631578947368,
-5.29999999999999));
#27364=CARTESIAN_POINT('Ctrl Pts',(1.42013071988495,40.4605263157895,-5.29999999999999));
#27365=CARTESIAN_POINT('Ctrl Pts',(2.64999999999999,40.6578947368421,-4.58993464005752));
#27366=CARTESIAN_POINT('Ctrl Pts',(3.87986928011504,40.8552631578947,-3.87986928011505));
#27367=CARTESIAN_POINT('Ctrl Pts',(4.58993464005751,41.0526315789473,-2.65));
#27368=CARTESIAN_POINT('Ctrl Pts',(5.29999999999999,41.25,-1.42013071988495));
#27369=CARTESIAN_POINT('Ctrl Pts',(5.29999999999999,41.4473684210526,-9.73594205322072E-16));
#27370=CARTESIAN_POINT('Ctrl Pts',(5.29999999999999,41.6447368421053,1.42013071988495));
#27371=CARTESIAN_POINT('Ctrl Pts',(4.58993464005752,41.8421052631579,2.64999999999999));
#27372=CARTESIAN_POINT('Ctrl Pts',(3.87986928011505,42.0394736842106,3.87986928011504));
#27373=CARTESIAN_POINT('Ctrl Pts',(2.65,42.2368421052632,4.58993464005751));
#27374=CARTESIAN_POINT('Ctrl Pts',(1.42013071988495,42.4342105263158,5.29999999999999));
#27375=CARTESIAN_POINT('Ctrl Pts',(4.99201041585172E-28,42.6315789473684,
5.29999999999999));
#27376=CARTESIAN_POINT('Ctrl Pts',(-1.42013071988495,42.8289473684211,5.29999999999998));
#27377=CARTESIAN_POINT('Ctrl Pts',(-2.65,43.0263157894737,4.58993464005752));
#27378=CARTESIAN_POINT('Ctrl Pts',(-3.87986928011504,43.2236842105263,3.87986928011504));
#27379=CARTESIAN_POINT('Ctrl Pts',(-4.58993464005751,43.421052631579,2.65));
#27380=CARTESIAN_POINT('Ctrl Pts',(-5.29999999999999,43.6184210526316,1.42013071988495));
#27381=CARTESIAN_POINT('Ctrl Pts',(-5.29999999999999,43.8157894736842,3.24531401774024E-16));
#27382=CARTESIAN_POINT('Ctrl Pts',(-5.29999999999999,44.0131578947368,-1.42013071988495));
#27383=CARTESIAN_POINT('Ctrl Pts',(-4.58993464005751,44.2105263157895,-2.64999999999999));
#27384=CARTESIAN_POINT('Ctrl Pts',(-3.87986928011504,44.4078947368421,-3.87986928011504));
#27385=CARTESIAN_POINT('Ctrl Pts',(-2.65,44.6052631578947,-4.58993464005751));
#27386=CARTESIAN_POINT('Ctrl Pts',(-1.42013071988495,44.8026315789473,-5.29999999999999));
#27387=CARTESIAN_POINT('Ctrl Pts',(-6.49062803547635E-16,45.,-5.29999999999999));
#27388=CARTESIAN_POINT('Ctrl Pts',(1.42013071988495,45.1973684210526,-5.29999999999999));
#27389=CARTESIAN_POINT('Ctrl Pts',(2.64999999999999,45.3947368421053,-4.58993464005752));
#27390=CARTESIAN_POINT('Ctrl Pts',(3.87986928011504,45.5921052631579,-3.87986928011505));
#27391=CARTESIAN_POINT('Ctrl Pts',(4.58993464005751,45.7894736842105,-2.65));
#27392=CARTESIAN_POINT('Ctrl Pts',(5.29999999999999,45.9868421052631,-1.42013071988495));
#27393=CARTESIAN_POINT('Ctrl Pts',(5.29999999999999,46.1842105263158,-9.73594205321085E-16));
#27394=CARTESIAN_POINT('Ctrl Pts',(5.29999999999999,46.3815789473684,1.42013071988495));
#27395=CARTESIAN_POINT('Ctrl Pts',(4.58993464005752,46.5789473684211,2.64999999999999));
#27396=CARTESIAN_POINT('Ctrl Pts',(3.87986928011505,46.7763157894737,3.87986928011504));
#27397=CARTESIAN_POINT('Ctrl Pts',(2.65,46.9736842105263,4.58993464005752));
#27398=CARTESIAN_POINT('Ctrl Pts',(1.42013071988495,47.1710526315789,5.29999999999999));
#27399=CARTESIAN_POINT('Ctrl Pts',(5.54667823983524E-28,47.3684210526316,
5.29999999999999));
#27400=CARTESIAN_POINT('Ctrl Pts',(-1.42013071988495,47.5657894736842,5.29999999999998));
#27401=CARTESIAN_POINT('Ctrl Pts',(-2.65,47.7631578947368,4.58993464005752));
#27402=CARTESIAN_POINT('Ctrl Pts',(-3.87986928011504,47.9605263157895,3.87986928011504));
#27403=CARTESIAN_POINT('Ctrl Pts',(-4.58993464005751,48.1578947368421,2.65));
#27404=CARTESIAN_POINT('Ctrl Pts',(-5.29999999999999,48.3552631578947,1.42013071988495));
#27405=CARTESIAN_POINT('Ctrl Pts',(-5.29999999999999,48.5526315789474,3.24531401773827E-16));
#27406=CARTESIAN_POINT('Ctrl Pts',(-5.29999999999999,48.75,-1.42013071988495));
#27407=CARTESIAN_POINT('Ctrl Pts',(-4.58993464005751,48.9473684210526,-2.64999999999999));
#27408=CARTESIAN_POINT('Ctrl Pts',(-3.87986928011504,49.1447368421053,-3.87986928011504));
#27409=CARTESIAN_POINT('Ctrl Pts',(-2.65,49.3421052631579,-4.58993464005751));
#27410=CARTESIAN_POINT('Ctrl Pts',(-1.42013071988495,49.5394736842105,-5.29999999999999));
#27411=CARTESIAN_POINT('Ctrl Pts',(-6.49062803547579E-16,49.7368421052631,
-5.29999999999999));
#27412=CARTESIAN_POINT('Ctrl Pts',(1.42013071988495,49.9342105263158,-5.29999999999999));
#27413=CARTESIAN_POINT('Ctrl Pts',(2.64999999999999,50.1315789473684,-4.58993464005752));
#27414=CARTESIAN_POINT('Ctrl Pts',(3.87986928011504,50.328947368421,-3.87986928011505));
#27415=CARTESIAN_POINT('Ctrl Pts',(4.58993464005751,50.5263157894737,-2.65));
#27416=CARTESIAN_POINT('Ctrl Pts',(5.29999999999999,50.7236842105263,-1.42013071988495));
#27417=CARTESIAN_POINT('Ctrl Pts',(5.29999999999999,50.9210526315789,-9.73594205321085E-16));
#27418=CARTESIAN_POINT('Ctrl Pts',(5.29999999999999,51.1184210526316,1.42013071988495));
#27419=CARTESIAN_POINT('Ctrl Pts',(4.58993464005752,51.3157894736842,2.64999999999999));
#27420=CARTESIAN_POINT('Ctrl Pts',(3.87986928011505,51.5131578947368,3.87986928011504));
#27421=CARTESIAN_POINT('Ctrl Pts',(2.65,51.7105263157895,4.58993464005752));
#27422=CARTESIAN_POINT('Ctrl Pts',(1.42013071988495,51.9078947368421,5.29999999999998));
#27423=CARTESIAN_POINT('Ctrl Pts',(6.00890142648818E-28,52.1052631578948,
5.29999999999999));
#27424=CARTESIAN_POINT('Ctrl Pts',(-1.42013071988495,52.3026315789474,5.29999999999999));
#27425=CARTESIAN_POINT('Ctrl Pts',(-2.65,52.5,4.58993464005752));
#27426=CARTESIAN_POINT('Ctrl Pts',(-3.87986928011504,52.6973684210526,3.87986928011504));
#27427=CARTESIAN_POINT('Ctrl Pts',(-4.58993464005751,52.8947368421053,2.65));
#27428=CARTESIAN_POINT('Ctrl Pts',(-5.29999999999999,53.0921052631579,1.42013071988495));
#27429=CARTESIAN_POINT('Ctrl Pts',(-5.29999999999999,53.2894736842105,3.245314017757E-16));
#27430=CARTESIAN_POINT('Ctrl Pts',(-5.29999999999999,53.4868421052631,-1.42013071988495));
#27431=CARTESIAN_POINT('Ctrl Pts',(-4.58993464005751,53.6842105263158,-2.64999999999999));
#27432=CARTESIAN_POINT('Ctrl Pts',(-3.87986928011504,53.8815789473684,-3.87986928011504));
#27433=CARTESIAN_POINT('Ctrl Pts',(-2.65,54.0789473684211,-4.58993464005751));
#27434=CARTESIAN_POINT('Ctrl Pts',(-1.42013071988495,54.2763157894737,-5.29999999999999));
#27435=CARTESIAN_POINT('Ctrl Pts',(-6.4906280354753E-16,54.4736842105263,
-5.29999999999999));
#27436=CARTESIAN_POINT('Ctrl Pts',(1.42013071988495,54.6710526315789,-5.29999999999999));
#27437=CARTESIAN_POINT('Ctrl Pts',(2.64999999999999,54.8684210526316,-4.58993464005752));
#27438=CARTESIAN_POINT('Ctrl Pts',(3.87986928011504,55.0657894736842,-3.87986928011505));
#27439=CARTESIAN_POINT('Ctrl Pts',(4.58993464005751,55.2631578947368,-2.65));
#27440=CARTESIAN_POINT('Ctrl Pts',(5.29999999999999,55.4605263157895,-1.42013071988495));
#27441=CARTESIAN_POINT('Ctrl Pts',(5.29999999999999,55.6578947368421,-9.73594205321578E-16));
#27442=CARTESIAN_POINT('Ctrl Pts',(5.29999999999999,55.8552631578947,1.42013071988495));
#27443=CARTESIAN_POINT('Ctrl Pts',(4.58993464005752,56.0526315789474,2.64999999999999));
#27444=CARTESIAN_POINT('Ctrl Pts',(3.87986928011505,56.25,3.87986928011504));
#27445=CARTESIAN_POINT('Ctrl Pts',(2.65,56.4473684210526,4.58993464005752));
#27446=CARTESIAN_POINT('Ctrl Pts',(1.42013071988495,56.6447368421052,5.29999999999999));
#27447=CARTESIAN_POINT('Ctrl Pts',(6.5635692504717E-28,56.8421052631579,
5.29999999999999));
#27448=CARTESIAN_POINT('Ctrl Pts',(-1.42013071988495,57.0394736842105,5.29999999999998));
#27449=CARTESIAN_POINT('Ctrl Pts',(-2.65,57.2368421052632,4.58993464005752));
#27450=CARTESIAN_POINT('Ctrl Pts',(-3.87986928011504,57.4342105263158,3.87986928011504));
#27451=CARTESIAN_POINT('Ctrl Pts',(-4.58993464005751,57.6315789473684,2.65));
#27452=CARTESIAN_POINT('Ctrl Pts',(-5.29999999999999,57.8289473684211,1.42013071988495));
#27453=CARTESIAN_POINT('Ctrl Pts',(-5.29999999999999,58.0263157894737,3.24531401775207E-16));
#27454=CARTESIAN_POINT('Ctrl Pts',(-5.29999999999999,58.2236842105263,-1.42013071988495));
#27455=CARTESIAN_POINT('Ctrl Pts',(-4.58993464005751,58.4210526315789,-2.64999999999999));
#27456=CARTESIAN_POINT('Ctrl Pts',(-3.87986928011504,58.6184210526315,-3.87986928011504));
#27457=CARTESIAN_POINT('Ctrl Pts',(-2.65,58.8157894736842,-4.58993464005751));
#27458=CARTESIAN_POINT('Ctrl Pts',(-1.42013071988495,59.0131578947368,-5.29999999999999));
#27459=CARTESIAN_POINT('Ctrl Pts',(-6.49062803547473E-16,59.2105263157894,
-5.29999999999999));
#27460=CARTESIAN_POINT('Ctrl Pts',(1.42013071988495,59.4078947368421,-5.29999999999999));
#27461=CARTESIAN_POINT('Ctrl Pts',(2.64999999999999,59.6052631578947,-4.58993464005752));
#27462=CARTESIAN_POINT('Ctrl Pts',(3.87986928011504,59.8026315789473,-3.87986928011505));
#27463=CARTESIAN_POINT('Ctrl Pts',(4.58993464005751,60.,-2.65));
#27464=CARTESIAN_POINT('Ctrl Pts',(5.29999999999999,60.1973684210526,-1.42013071988495));
#27465=CARTESIAN_POINT('Ctrl Pts',(5.29999999999999,60.3947368421052,-9.73594205321184E-16));
#27466=CARTESIAN_POINT('Ctrl Pts',(5.29999999999999,60.5921052631579,1.42013071988495));
#27467=CARTESIAN_POINT('Ctrl Pts',(4.58993464005752,60.7894736842105,2.64999999999999));
#27468=CARTESIAN_POINT('Ctrl Pts',(3.87986928011505,60.9868421052632,3.87986928011504));
#27469=CARTESIAN_POINT('Ctrl Pts',(2.65,61.1842105263158,4.58993464005752));
#27470=CARTESIAN_POINT('Ctrl Pts',(1.42013071988495,61.3815789473684,5.29999999999998));
#27471=CARTESIAN_POINT('Ctrl Pts',(7.02579243712464E-28,61.5789473684211,
5.29999999999999));
#27472=CARTESIAN_POINT('Ctrl Pts',(-1.42013071988495,61.7763157894737,5.29999999999999));
#27473=CARTESIAN_POINT('Ctrl Pts',(-2.65,61.9736842105264,4.58993464005752));
#27474=CARTESIAN_POINT('Ctrl Pts',(-3.87986928011504,62.171052631579,3.87986928011505));
#27475=CARTESIAN_POINT('Ctrl Pts',(-4.58993464005751,62.3684210526316,2.65));
#27476=CARTESIAN_POINT('Ctrl Pts',(-5.29999999999999,62.5657894736842,1.42013071988495));
#27477=CARTESIAN_POINT('Ctrl Pts',(-5.29999999999999,62.7631578947368,3.24531401775109E-16));
#27478=CARTESIAN_POINT('Ctrl Pts',(-5.29999999999999,62.9605263157895,-1.42013071988495));
#27479=CARTESIAN_POINT('Ctrl Pts',(-4.58993464005751,63.1578947368421,-2.64999999999999));
#27480=CARTESIAN_POINT('Ctrl Pts',(-3.87986928011504,63.3552631578947,-3.87986928011504));
#27481=CARTESIAN_POINT('Ctrl Pts',(-2.65,63.5526315789474,-4.58993464005751));
#27482=CARTESIAN_POINT('Ctrl Pts',(-1.42013071988495,63.75,-5.29999999999999));
#27483=CARTESIAN_POINT('Ctrl Pts',(-6.49062803547422E-16,63.9473684210526,
-5.29999999999999));
#27484=CARTESIAN_POINT('Ctrl Pts',(1.42013071988495,64.1447368421053,-5.29999999999999));
#27485=CARTESIAN_POINT('Ctrl Pts',(2.64999999999999,64.3421052631579,-4.58993464005752));
#27486=CARTESIAN_POINT('Ctrl Pts',(3.87986928011504,64.5394736842105,-3.87986928011505));
#27487=CARTESIAN_POINT('Ctrl Pts',(4.58993464005751,64.7368421052632,-2.65));
#27488=CARTESIAN_POINT('Ctrl Pts',(5.29999999999999,64.9342105263157,-1.42013071988495));
#27489=CARTESIAN_POINT('Ctrl Pts',(5.29999999999999,65.1315789473684,-9.73594205320987E-16));
#27490=CARTESIAN_POINT('Ctrl Pts',(5.29999999999999,65.328947368421,1.42013071988495));
#27491=CARTESIAN_POINT('Ctrl Pts',(4.58993464005752,65.5263157894737,2.64999999999999));
#27492=CARTESIAN_POINT('Ctrl Pts',(3.87986928011505,65.7236842105264,3.87986928011504));
#27493=CARTESIAN_POINT('Ctrl Pts',(2.65,65.9210526315789,4.58993464005752));
#27494=CARTESIAN_POINT('Ctrl Pts',(1.42013071988495,66.1184210526315,5.29999999999999));
#27495=CARTESIAN_POINT('Ctrl Pts',(7.48801562377757E-28,66.3157894736842,
5.29999999999999));
#27496=CARTESIAN_POINT('Ctrl Pts',(-1.42013071988495,66.5131578947368,5.29999999999998));
#27497=CARTESIAN_POINT('Ctrl Pts',(-2.65,66.7105263157894,4.58993464005752));
#27498=CARTESIAN_POINT('Ctrl Pts',(-3.87986928011504,66.9078947368421,3.87986928011504));
#27499=CARTESIAN_POINT('Ctrl Pts',(-4.58993464005751,67.1052631578947,2.65));
#27500=CARTESIAN_POINT('Ctrl Pts',(-5.29999999999999,67.3026315789474,1.42013071988495));
#27501=CARTESIAN_POINT('Ctrl Pts',(-5.29999999999999,67.5,3.24531401774714E-16));
#27502=CARTESIAN_POINT('Ctrl Pts',(-5.29999999999999,67.6973684210526,-1.42013071988495));
#27503=CARTESIAN_POINT('Ctrl Pts',(-4.58993464005751,67.8947368421052,-2.64999999999999));
#27504=CARTESIAN_POINT('Ctrl Pts',(-3.87986928011504,68.0921052631578,-3.87986928011504));
#27505=CARTESIAN_POINT('Ctrl Pts',(-2.65,68.2894736842105,-4.58993464005751));
#27506=CARTESIAN_POINT('Ctrl Pts',(-1.42013071988495,68.4868421052632,-5.29999999999999));
#27507=CARTESIAN_POINT('Ctrl Pts',(-6.49062803547376E-16,68.6842105263158,
-5.29999999999999));
#27508=CARTESIAN_POINT('Ctrl Pts',(1.42013071988495,68.8815789473684,-5.29999999999999));
#27509=CARTESIAN_POINT('Ctrl Pts',(2.64999999999999,69.078947368421,-4.58993464005752));
#27510=CARTESIAN_POINT('Ctrl Pts',(3.87986928011504,69.2763157894736,-3.87986928011505));
#27511=CARTESIAN_POINT('Ctrl Pts',(4.58993464005751,69.4736842105263,-2.65));
#27512=CARTESIAN_POINT('Ctrl Pts',(5.29999999999999,69.6710526315789,-1.42013071988495));
#27513=CARTESIAN_POINT('Ctrl Pts',(5.29999999999999,69.8684210526316,-9.73594205320888E-16));
#27514=CARTESIAN_POINT('Ctrl Pts',(5.29999999999999,70.0657894736842,1.42013071988495));
#27515=CARTESIAN_POINT('Ctrl Pts',(4.58993464005752,70.2631578947369,2.64999999999999));
#27516=CARTESIAN_POINT('Ctrl Pts',(3.87986928011505,70.4605263157895,3.87986928011504));
#27517=CARTESIAN_POINT('Ctrl Pts',(2.65,70.6578947368421,4.58993464005752));
#27518=CARTESIAN_POINT('Ctrl Pts',(1.42013071988495,70.8552631578947,5.29999999999998));
#27519=CARTESIAN_POINT('Ctrl Pts',(7.96564624998561E-28,71.0526315789473,
5.29999999999999));
#27520=CARTESIAN_POINT('Ctrl Pts',(-1.42013071988495,71.2499999999999,5.29999999999999));
#27521=CARTESIAN_POINT('Ctrl Pts',(-2.65,71.4473684210526,4.58993464005751));
#27522=CARTESIAN_POINT('Ctrl Pts',(-3.87986928011504,71.6447368421053,3.87986928011504));
#27523=CARTESIAN_POINT('Ctrl Pts',(-4.58993464005751,71.8421052631579,2.65));
#27524=CARTESIAN_POINT('Ctrl Pts',(-5.29999999999999,72.0394736842105,1.42013071988495));
#27525=CARTESIAN_POINT('Ctrl Pts',(-5.29999999999999,72.2368421052632,3.24531401775306E-16));
#27526=CARTESIAN_POINT('Ctrl Pts',(-5.29999999999999,72.4342105263157,-1.42013071988495));
#27527=CARTESIAN_POINT('Ctrl Pts',(-4.58993464005751,72.6315789473684,-2.64999999999999));
#27528=CARTESIAN_POINT('Ctrl Pts',(-3.87986928011504,72.828947368421,-3.87986928011504));
#27529=CARTESIAN_POINT('Ctrl Pts',(-2.65,73.0263157894737,-4.58993464005751));
#27530=CARTESIAN_POINT('Ctrl Pts',(-1.42013071988495,73.2236842105263,-5.29999999999999));
#27531=CARTESIAN_POINT('Ctrl Pts',(-6.4906280354732E-16,73.421052631579,
-5.29999999999999));
#27532=CARTESIAN_POINT('Ctrl Pts',(1.42013071988495,73.6184210526315,-5.29999999999999));
#27533=CARTESIAN_POINT('Ctrl Pts',(2.64999999999999,73.8157894736842,-4.58993464005751));
#27534=CARTESIAN_POINT('Ctrl Pts',(3.87986928011504,74.0131578947368,-3.87986928011505));
#27535=CARTESIAN_POINT('Ctrl Pts',(4.58993464005751,74.2105263157895,-2.65));
#27536=CARTESIAN_POINT('Ctrl Pts',(5.29999999999999,74.4078947368421,-1.42013071988495));
#27537=CARTESIAN_POINT('Ctrl Pts',(5.29999999999999,74.6052631578947,-9.73594205321085E-16));
#27538=CARTESIAN_POINT('Ctrl Pts',(5.29999999999999,74.8026315789473,1.42013071988495));
#27539=CARTESIAN_POINT('Ctrl Pts',(4.58993464005752,75.,2.64999999999999));
#27540=CARTESIAN_POINT('Ctrl Pts',(3.87986928011505,75.1973684210526,3.87986928011504));
#27541=CARTESIAN_POINT('Ctrl Pts',(2.65,75.3947368421052,4.58993464005751));
#27542=CARTESIAN_POINT('Ctrl Pts',(1.42013071988495,75.5921052631578,5.29999999999998));
#27543=CARTESIAN_POINT('Ctrl Pts',(8.68979590907521E-28,75.7894736842105,
5.29999999999999));
#27544=CARTESIAN_POINT('Ctrl Pts',(-1.42013071988495,75.9868421052631,5.29999999999999));
#27545=CARTESIAN_POINT('Ctrl Pts',(-2.65,76.1842105263158,4.58993464005751));
#27546=CARTESIAN_POINT('Ctrl Pts',(-3.87986928011504,76.3815789473684,3.87986928011504));
#27547=CARTESIAN_POINT('Ctrl Pts',(-4.58993464005751,76.5789473684211,2.65));
#27548=CARTESIAN_POINT('Ctrl Pts',(-5.29999999999999,76.7763157894737,1.42013071988495));
#27549=CARTESIAN_POINT('Ctrl Pts',(-5.29999999999999,76.9736842105263,3.24531401774615E-16));
#27550=CARTESIAN_POINT('Ctrl Pts',(-5.29999999999999,77.1710526315789,-1.42013071988495));
#27551=CARTESIAN_POINT('Ctrl Pts',(-4.58993464005751,77.3684210526315,-2.64999999999999));
#27552=CARTESIAN_POINT('Ctrl Pts',(-3.87986928011504,77.5657894736842,-3.87986928011504));
#27553=CARTESIAN_POINT('Ctrl Pts',(-2.65,77.7631578947368,-4.58993464005751));
#27554=CARTESIAN_POINT('Ctrl Pts',(-1.42013071988495,77.9605263157895,-5.29999999999999));
#27555=CARTESIAN_POINT('Ctrl Pts',(-6.49062803547265E-16,78.1578947368421,
-5.29999999999999));
#27556=CARTESIAN_POINT('Ctrl Pts',(1.42013071988495,78.3552631578948,-5.29999999999999));
#27557=CARTESIAN_POINT('Ctrl Pts',(2.64999999999999,78.5526315789474,-4.58993464005751));
#27558=CARTESIAN_POINT('Ctrl Pts',(3.87986928011504,78.7499999999999,-3.87986928011505));
#27559=CARTESIAN_POINT('Ctrl Pts',(4.58993464005751,78.9473684210526,-2.65));
#27560=CARTESIAN_POINT('Ctrl Pts',(5.29999999999999,79.1447368421052,-1.42013071988495));
#27561=CARTESIAN_POINT('Ctrl Pts',(5.29999999999999,79.3421052631579,-9.73594205320987E-16));
#27562=CARTESIAN_POINT('Ctrl Pts',(5.29999999999999,79.5394736842105,1.42013071988495));
#27563=CARTESIAN_POINT('Ctrl Pts',(4.58993464005752,79.7368421052632,2.64999999999999));
#27564=CARTESIAN_POINT('Ctrl Pts',(3.87986928011505,79.9342105263158,3.87986928011504));
#27565=CARTESIAN_POINT('Ctrl Pts',(2.65,80.1315789473684,4.58993464005751));
#27566=CARTESIAN_POINT('Ctrl Pts',(1.42013071988495,80.328947368421,5.29999999999999));
#27567=CARTESIAN_POINT('Ctrl Pts',(9.15201909572814E-28,80.5263157894736,
5.3));
#27568=CARTESIAN_POINT('Ctrl Pts',(-1.42013071988495,80.7236842105263,5.29999999999998));
#27569=CARTESIAN_POINT('Ctrl Pts',(-2.65,80.9210526315789,4.58993464005751));
#27570=CARTESIAN_POINT('Ctrl Pts',(-3.87986928011504,81.1184210526315,3.87986928011504));
#27571=CARTESIAN_POINT('Ctrl Pts',(-4.58993464005751,81.3157894736842,2.64999999999999));
#27572=CARTESIAN_POINT('Ctrl Pts',(-5.29999999999999,81.5131578947368,1.42013071988495));
#27573=CARTESIAN_POINT('Ctrl Pts',(-5.29999999999999,81.7105263157895,3.24531401775207E-16));
#27574=CARTESIAN_POINT('Ctrl Pts',(-5.29999999999999,81.9078947368421,-1.42013071988495));
#27575=CARTESIAN_POINT('Ctrl Pts',(-4.58993464005751,82.1052631578947,-2.64999999999999));
#27576=CARTESIAN_POINT('Ctrl Pts',(-3.87986928011504,82.3026315789473,-3.87986928011504));
#27577=CARTESIAN_POINT('Ctrl Pts',(-2.65,82.5,-4.58993464005751));
#27578=CARTESIAN_POINT('Ctrl Pts',(-1.42013071988495,82.6973684210527,-5.29999999999999));
#27579=CARTESIAN_POINT('Ctrl Pts',(-6.49062803547219E-16,82.8947368421053,
-5.29999999999999));
#27580=CARTESIAN_POINT('Ctrl Pts',(1.42013071988495,83.0921052631579,-5.29999999999999));
#27581=CARTESIAN_POINT('Ctrl Pts',(2.64999999999999,83.2894736842105,-4.58993464005751));
#27582=CARTESIAN_POINT('Ctrl Pts',(3.87986928011504,83.4868421052631,-3.87986928011505));
#27583=CARTESIAN_POINT('Ctrl Pts',(4.58993464005751,83.6842105263158,-2.65));
#27584=CARTESIAN_POINT('Ctrl Pts',(5.29999999999999,83.8815789473684,-1.42013071988495));
#27585=CARTESIAN_POINT('Ctrl Pts',(5.29999999999999,84.078947368421,-9.73594205321184E-16));
#27586=CARTESIAN_POINT('Ctrl Pts',(5.29999999999999,84.2763157894736,1.42013071988495));
#27587=CARTESIAN_POINT('Ctrl Pts',(4.58993464005752,84.4736842105263,2.64999999999999));
#27588=CARTESIAN_POINT('Ctrl Pts',(3.87986928011505,84.6710526315789,3.87986928011504));
#27589=CARTESIAN_POINT('Ctrl Pts',(2.65,84.8684210526316,4.58993464005751));
#27590=CARTESIAN_POINT('Ctrl Pts',(1.42013071988495,85.0657894736842,5.29999999999998));
#27591=CARTESIAN_POINT('Ctrl Pts',(9.61424228238108E-28,85.2631578947368,
5.3));
#27592=CARTESIAN_POINT('Ctrl Pts',(-1.42013071988495,85.4605263157894,5.29999999999999));
#27593=CARTESIAN_POINT('Ctrl Pts',(-2.65,85.6578947368421,4.58993464005751));
#27594=CARTESIAN_POINT('Ctrl Pts',(-3.87986928011504,85.8552631578947,3.87986928011504));
#27595=CARTESIAN_POINT('Ctrl Pts',(-4.58993464005751,86.0526315789474,2.65));
#27596=CARTESIAN_POINT('Ctrl Pts',(-5.29999999999999,86.25,1.42013071988495));
#27597=CARTESIAN_POINT('Ctrl Pts',(-5.29999999999999,86.4473684210526,3.24531401775207E-16));
#27598=CARTESIAN_POINT('Ctrl Pts',(-5.29999999999999,86.6447368421052,-1.42013071988495));
#27599=CARTESIAN_POINT('Ctrl Pts',(-4.58993464005751,86.8421052631579,-2.64999999999999));
#27600=CARTESIAN_POINT('Ctrl Pts',(-3.87986928011504,87.0394736842105,-3.87986928011504));
#27601=CARTESIAN_POINT('Ctrl Pts',(-2.65,87.2368421052631,-4.58993464005751));
#27602=CARTESIAN_POINT('Ctrl Pts',(-1.42013071988495,87.4342105263158,-5.29999999999999));
#27603=CARTESIAN_POINT('Ctrl Pts',(-6.49062803547173E-16,87.6315789473684,
-5.29999999999999));
#27604=CARTESIAN_POINT('Ctrl Pts',(1.42013071988495,87.828947368421,-5.29999999999999));
#27605=CARTESIAN_POINT('Ctrl Pts',(2.64999999999999,88.0263157894737,-4.58993464005751));
#27606=CARTESIAN_POINT('Ctrl Pts',(3.87986928011504,88.2236842105263,-3.87986928011505));
#27607=CARTESIAN_POINT('Ctrl Pts',(4.58993464005751,88.4210526315789,-2.65));
#27608=CARTESIAN_POINT('Ctrl Pts',(5.29999999999999,88.6184210526316,-1.42013071988495));
#27609=CARTESIAN_POINT('Ctrl Pts',(5.29999999999999,88.8157894736842,-9.73594205321085E-16));
#27610=CARTESIAN_POINT('Ctrl Pts',(5.29999999999999,89.0131578947368,1.42013071988495));
#27611=CARTESIAN_POINT('Ctrl Pts',(4.58993464005752,89.2105263157895,2.64999999999999));
#27612=CARTESIAN_POINT('Ctrl Pts',(3.87986928011505,89.4078947368421,3.87986928011504));
#27613=CARTESIAN_POINT('Ctrl Pts',(2.65,89.6052631578947,4.58993464005751));
#27614=CARTESIAN_POINT('Ctrl Pts',(1.42013071988495,89.8026315789473,5.29999999999999));
#27615=CARTESIAN_POINT('Ctrl Pts',(1.01689101063646E-27,89.9999999999999,
5.3));
#27616=CARTESIAN_POINT('Ctrl Pts',(-1.11022302462516E-15,90.,5.3));
#27617=CARTESIAN_POINT('Ctrl Pts',(0.705100735517942,90.,5.29999999999999));
#27618=CARTESIAN_POINT('Ctrl Pts',(1.4049232938638,90.,5.16650652249293));
#27619=CARTESIAN_POINT('Ctrl Pts',(2.30127966598412,90.,4.81265289415681));
#27620=CARTESIAN_POINT('Ctrl Pts',(2.53381374000113,90.,4.70178046144737));
#27621=CARTESIAN_POINT('Ctrl Pts',(3.38128440167258,90.,4.22331897236908));
#27622=CARTESIAN_POINT('Ctrl Pts',(3.93207008557601,90.,3.75829552364623));
#27623=CARTESIAN_POINT('Ctrl Pts',(4.62745111738881,90.,2.90535644419948));
#27624=CARTESIAN_POINT('Ctrl Pts',(4.84005013405767,90.,2.58173505428712));
#27625=CARTESIAN_POINT('Ctrl Pts',(5.20015385755245,90.,1.9003141675501));
#27626=CARTESIAN_POINT('Ctrl Pts',(5.3477175335123,90.,1.53988706209255));
#27627=CARTESIAN_POINT('Ctrl Pts',(5.73877457275006,90.,0.239224399660193));
#27628=CARTESIAN_POINT('Ctrl Pts',(5.75207974392297,90.,-0.612754734201201));
#27629=CARTESIAN_POINT('Ctrl Pts',(5.58692017936483,90.,-2.20371577024327));
#27630=CARTESIAN_POINT('Ctrl Pts',(5.30528429685785,90.,-3.05722906998427));
#27631=CARTESIAN_POINT('Ctrl Pts',(4.41388010965142,90.,-4.76270163974273));
#27632=CARTESIAN_POINT('Ctrl Pts',(3.88988452656918,90.0000000000059,-5.3939572843751));
#27633=CARTESIAN_POINT('Ctrl Pts',(3.51744452299761,90.0000000000059,-5.97932511428333));
#27634=CARTESIAN_POINT('Ctrl Pts',(3.46100601870892,90.,-6.08614105674003));
#27635=CARTESIAN_POINT('Ctrl Pts',(3.41267186745819,90.,-6.22249169412421));
#27636=CARTESIAN_POINT('Ctrl Pts',(3.39968442225245,90.,-6.27278714382266));
#27637=CARTESIAN_POINT('Ctrl Pts',(3.39615776458109,90.,-6.35191890437968));
#27638=CARTESIAN_POINT('Ctrl Pts',(3.3988649016033,90.,-6.38210532885075));
#27639=CARTESIAN_POINT('Ctrl Pts',(3.41578433719734,90.,-6.43733794772286));
#27640=CARTESIAN_POINT('Ctrl Pts',(3.4285533280344,90.0000000000201,-6.4611916715849));
#27641=CARTESIAN_POINT('Ctrl Pts',(3.4673290106001,90.0000000000201,-6.50808285636127));
#27642=CARTESIAN_POINT('Ctrl Pts',(3.49403994958472,90.0000000000001,-6.52813135760766));
#27643=CARTESIAN_POINT('Ctrl Pts',(3.57279538848092,90.0000000000001,-6.57029447033136));
#27644=CARTESIAN_POINT('Ctrl Pts',(3.63078887712831,90.,-6.58503381585687));
#27645=CARTESIAN_POINT('Ctrl Pts',(3.79711934339588,90.,-6.60906710879125));
#27646=CARTESIAN_POINT('Ctrl Pts',(3.92236333330237,90.,-6.6017658708962));
#27647=CARTESIAN_POINT('Ctrl Pts',(4.35612042347956,90.,-6.54400669481274));
#27648=CARTESIAN_POINT('Ctrl Pts',(4.78534531728318,90.0000000000001,-6.40675881673715));
#27649=CARTESIAN_POINT('Ctrl Pts',(5.85107880669982,90.0000000000001,-5.83387569838342));
#27650=CARTESIAN_POINT('Ctrl Pts',(6.48172283195264,90.,-5.34839112546546));
#27651=CARTESIAN_POINT('Ctrl Pts',(7.64464329931856,90.,-3.9916659757713));
#27652=CARTESIAN_POINT('Ctrl Pts',(8.17812076497661,90.,-3.10007009428681));
#27653=CARTESIAN_POINT('Ctrl Pts',(8.90148181129173,90.,-0.887883537440906));
#27654=CARTESIAN_POINT('Ctrl Pts',(8.98096602140476,89.9999999997875,0.240626946476822));
#27655=CARTESIAN_POINT('Ctrl Pts',(8.80307772603727,89.9999999997875,2.35592379430447));
#27656=CARTESIAN_POINT('Ctrl Pts',(8.48937235653017,90.,3.44640186127508));
#27657=CARTESIAN_POINT('Ctrl Pts',(7.84903191346606,90.,4.69681107334978));
#27658=CARTESIAN_POINT('Ctrl Pts',(7.70886753716707,90.,4.94099545221441));
#27659=CARTESIAN_POINT('Ctrl Pts',(6.95641557015424,90.,6.11888992491444));
#27660=CARTESIAN_POINT('Ctrl Pts',(6.18323092075226,90.,6.93754127757638));
#27661=CARTESIAN_POINT('Ctrl Pts',(4.86855345588626,90.,7.88920095492676));
#27662=CARTESIAN_POINT('Ctrl Pts',(4.43381295061861,90.,8.15052437235101));
#27663=CARTESIAN_POINT('Ctrl Pts',(3.34564146975116,90.,8.68638626613442));
#27664=CARTESIAN_POINT('Ctrl Pts',(2.67551791995553,89.9999999999999,8.92322547450994));
#27665=CARTESIAN_POINT('Ctrl Pts',(1.65577548687742,89.9999999999999,9.15323079586583));
#27666=CARTESIAN_POINT('Ctrl Pts',(1.32324826699197,89.9999999999954,9.20885494539258));
#27667=CARTESIAN_POINT('Ctrl Pts',(0.660151381649946,89.9999999999954,9.28190034665736));
#27668=CARTESIAN_POINT('Ctrl Pts',(0.330207854361134,90.,9.29999999999998));
#27669=CARTESIAN_POINT('Ctrl Pts',(1.17961196366423E-14,90.,9.29999999999998));
#27670=CARTESIAN_POINT('Ctrl Pts',(-3.46944695195361E-17,-3.22290425329321E-15,
5.29999999999999));
#27671=CARTESIAN_POINT('Ctrl Pts',(-0.169644532845145,-3.22267314244815E-15,
5.29999999999999));
#27672=CARTESIAN_POINT('Ctrl Pts',(-0.339214759582775,1.69602044929706E-12,
5.2922718595307));
#27673=CARTESIAN_POINT('Ctrl Pts',(-0.680184164497541,1.69602044929706E-12,
5.26118280144906));
#27674=CARTESIAN_POINT('Ctrl Pts',(-0.851408033835457,-2.72945075257972E-15,
5.23755326103085));
#27675=CARTESIAN_POINT('Ctrl Pts',(-1.37651569900196,-2.70949669069754E-15,
5.14023686030182));
#27676=CARTESIAN_POINT('Ctrl Pts',(-1.72474458805228,-3.73063229218745E-15,
5.04025101866987));
#27677=CARTESIAN_POINT('Ctrl Pts',(-2.30127966599588,-3.70905464750116E-15,
4.81265289415161));
#27678=CARTESIAN_POINT('Ctrl Pts',(-2.53381374001407,-3.36411559846784E-15,
4.70178046144089));
#27679=CARTESIAN_POINT('Ctrl Pts',(-3.38128440168497,-3.31624161775105E-15,
4.22331897235982));
#27680=CARTESIAN_POINT('Ctrl Pts',(-3.93207008558682,-3.10712189669725E-15,
3.75829552363584));
#27681=CARTESIAN_POINT('Ctrl Pts',(-4.62745111739741,-3.00622202880969E-15,
2.90535644418744));
#27682=CARTESIAN_POINT('Ctrl Pts',(-4.84005013406567,-2.86023292837575E-15,
2.58173505427411));
#27683=CARTESIAN_POINT('Ctrl Pts',(-5.20015385755875,-2.76909805416762E-15,
1.90031416753604));
#27684=CARTESIAN_POINT('Ctrl Pts',(-5.34771753351767,3.39051007573177E-14,
1.53988706207808));
#27685=CARTESIAN_POINT('Ctrl Pts',(-5.73877457275226,3.40242515497888E-14,
0.239224399644201));
#27686=CARTESIAN_POINT('Ctrl Pts',(-5.75207974392291,-3.39098433734155E-15,
-0.612754734217791));
#27687=CARTESIAN_POINT('Ctrl Pts',(-5.58692017936078,-3.20318749950661E-15,
-2.20371577025992));
#27688=CARTESIAN_POINT('Ctrl Pts',(-5.30528429685125,-2.68925673330566E-15,
-3.05722907000087));
#27689=CARTESIAN_POINT('Ctrl Pts',(-4.41388010964463,-2.49467807752504E-15,
-4.76270163975131));
#27690=CARTESIAN_POINT('Ctrl Pts',(-3.88988452656653,-5.92898608183421E-12,
-5.3939572843788));
#27691=CARTESIAN_POINT('Ctrl Pts',(-3.51744452299239,-5.92890982212414E-12,
-5.97932511429165));
#27692=CARTESIAN_POINT('Ctrl Pts',(-3.46100601870684,-2.78405185707395E-15,
-6.08614105674537));
#27693=CARTESIAN_POINT('Ctrl Pts',(-3.41267186745706,-2.76558424548778E-15,
-6.22249169412705));
#27694=CARTESIAN_POINT('Ctrl Pts',(-3.39968442225255,-2.23295764606424E-15,
-6.27278714382351));
#27695=CARTESIAN_POINT('Ctrl Pts',(-3.39615776458133,-2.22289674085925E-15,
-6.35191890437837));
#27696=CARTESIAN_POINT('Ctrl Pts',(-3.39886490160313,-3.34829527742224E-15,
-6.38210532885045));
#27697=CARTESIAN_POINT('Ctrl Pts',(-3.41578433719774,-3.34140661391927E-15,
-6.43733794772428));
#27698=CARTESIAN_POINT('Ctrl Pts',(-3.42855332803508,-2.0063968588949E-11,
-6.46119167158541));
#27699=CARTESIAN_POINT('Ctrl Pts',(-3.46732901060007,-2.00639629001137E-11,
-6.50808285636085));
#27700=CARTESIAN_POINT('Ctrl Pts',(-3.49403994958348,-2.22765705204529E-15,
-6.52813135760707));
#27701=CARTESIAN_POINT('Ctrl Pts',(-3.57279538848081,-2.22376902594429E-15,
-6.5702944703313));
#27702=CARTESIAN_POINT('Ctrl Pts',(-3.63078887712726,-2.21658829378393E-15,
-6.58503381585689));
#27703=CARTESIAN_POINT('Ctrl Pts',(-3.79711934339621,-2.2129999729789E-15,
-6.60906710879137));
#27704=CARTESIAN_POINT('Ctrl Pts',(-3.9223633333031,-1.1011763607202E-15,
-6.60176587089621));
#27705=CARTESIAN_POINT('Ctrl Pts',(-4.35612042348101,-1.1011763607202E-15,
-6.54400669481249));
#27706=CARTESIAN_POINT('Ctrl Pts',(-4.78534531728578,-1.58613680503368E-15,
-6.40675881673634));
#27707=CARTESIAN_POINT('Ctrl Pts',(-5.85107880670852,-1.66733944063455E-15,
-5.83387569837821));
#27708=CARTESIAN_POINT('Ctrl Pts',(-6.48172283196021,-3.9730222950244E-15,
-5.34839112545779));
#27709=CARTESIAN_POINT('Ctrl Pts',(-7.64464329931948,-4.13836029449498E-15,
-3.99166597576912));
#27710=CARTESIAN_POINT('Ctrl Pts',(-8.17812076497821,-3.19046254333735E-15,
-3.10007009428486));
#27711=CARTESIAN_POINT('Ctrl Pts',(-8.90148181129361,-3.46494457383746E-15,
-0.887883537432394));
#27712=CARTESIAN_POINT('Ctrl Pts',(-8.98096602140475,2.12463464266943E-10,
0.240626946485903));
#27713=CARTESIAN_POINT('Ctrl Pts',(-8.8030777260359,2.12463194834947E-10,
2.3559237943109));
#27714=CARTESIAN_POINT('Ctrl Pts',(-8.48937235652788,-2.82135042331067E-15,
3.44640186128145));
#27715=CARTESIAN_POINT('Ctrl Pts',(-7.84903191346284,-2.94513386976895E-15,
4.69681107335558));
#27716=CARTESIAN_POINT('Ctrl Pts',(-7.70886753716375,-3.79933706437609E-15,
4.94099545221998));
#27717=CARTESIAN_POINT('Ctrl Pts',(-6.95641557015005,-3.92492878533535E-15,
6.11888992491946));
#27718=CARTESIAN_POINT('Ctrl Pts',(-6.18323092074754,-3.63640987014422E-15,
6.93754127758076));
#27719=CARTESIAN_POINT('Ctrl Pts',(-4.86855345588147,-3.72862351382448E-15,
7.88920095492979));
#27720=CARTESIAN_POINT('Ctrl Pts',(-4.4338129506142,-3.2452453412235E-15,
8.15052437235346));
#27721=CARTESIAN_POINT('Ctrl Pts',(-3.34564146974786,-3.30469395986477E-15,
8.68638626613567));
#27722=CARTESIAN_POINT('Ctrl Pts',(-2.67551791995298,-3.67618129863226E-15,
8.92322547451067));
#27723=CARTESIAN_POINT('Ctrl Pts',(-1.33313154318946,-3.71996106794212E-15,
9.22600390164642));
#27724=CARTESIAN_POINT('Ctrl Pts',(-0.667662034038393,-3.71105124528613E-15,
9.29999999999998));
#27725=CARTESIAN_POINT('Ctrl Pts',(1.38777878078145E-16,-3.71274633697002E-15,
9.29999999999998));
#27726=CARTESIAN_POINT('Origin',(-9.29999999999998,0.,-21.4633238078319));
#27727=CARTESIAN_POINT('Origin',(-9.29999999999998,90.,-21.4633238078319));
#27728=CARTESIAN_POINT('',(0.,0.,0.));
#27729=CARTESIAN_POINT('Origin',(0.,26.,0.));
#27730=CARTESIAN_POINT('',(0.,1.,9.15));
#27731=CARTESIAN_POINT('',(-1.12055182121983E-15,1.,-9.15));
#27732=CARTESIAN_POINT('Origin',(0.,1.,0.));
#27733=CARTESIAN_POINT('Origin',(0.,1.,0.));
#27734=CARTESIAN_POINT('',(0.,26.,9.15));
#27735=CARTESIAN_POINT('',(-1.12055182121983E-15,26.,9.15));
#27736=CARTESIAN_POINT('Origin',(0.,26.,0.));
#27737=CARTESIAN_POINT('Origin',(0.,26.,0.));
#27738=CARTESIAN_POINT('',(0.,26.,6.75));
#27739=CARTESIAN_POINT('Origin',(0.,26.,0.));
#27740=CARTESIAN_POINT('Origin',(0.,0.,0.));
#27741=CARTESIAN_POINT('',(-9.98087141305093E-16,0.,-8.15));
#27742=CARTESIAN_POINT('Origin',(0.,0.,0.));
#27743=CARTESIAN_POINT('',(0.,0.,-3.57071421427142));
#27744=CARTESIAN_POINT('Origin',(0.,0.,0.));
#27745=CARTESIAN_POINT('Origin',(0.,27.5,0.));
#27746=CARTESIAN_POINT('',(0.,27.5,6.75));
#27747=CARTESIAN_POINT('',(-8.26636589424463E-16,27.5,6.75));
#27748=CARTESIAN_POINT('Origin',(0.,27.5,0.));
#27749=CARTESIAN_POINT('Origin',(0.,27.5,0.));
#27750=CARTESIAN_POINT('',(-3.85,27.5,-3.81794919243112));
#27751=CARTESIAN_POINT('',(-3.85,27.5,3.81794919243112));
#27752=CARTESIAN_POINT('',(-3.85,27.5,3.55));
#27753=CARTESIAN_POINT('',(3.85,27.5,-3.81794919243112));
#27754=CARTESIAN_POINT('',(-4.30070525597205E-16,27.5,-3.81794919243112));
#27755=CARTESIAN_POINT('',(3.85,27.5,3.81794919243112));
#27756=CARTESIAN_POINT('',(3.85,27.5,3.55));
#27757=CARTESIAN_POINT('',(4.30070525597205E-16,27.5,3.81794919243112));
#27758=CARTESIAN_POINT('Origin',(-3.85,26.5,3.55));
#27759=CARTESIAN_POINT('',(-3.85,26.5,3.55));
#27760=CARTESIAN_POINT('',(-3.85,26.5,3.55));
#27761=CARTESIAN_POINT('',(-3.85,26.5,-3.55));
#27762=CARTESIAN_POINT('',(-3.85,26.5,3.55));
#27763=CARTESIAN_POINT('',(-3.85,26.5,-3.55));
#27764=CARTESIAN_POINT('Origin',(3.85,26.5,-3.55));
#27765=CARTESIAN_POINT('',(3.85,26.5,-3.55));
#27766=CARTESIAN_POINT('',(3.85,26.5,-3.55));
#27767=CARTESIAN_POINT('',(3.85,24.725,-3.07439018343476));
#27768=CARTESIAN_POINT('Origin',(3.85,26.5,3.55));
#27769=CARTESIAN_POINT('',(3.85,26.5,3.55));
#27770=CARTESIAN_POINT('',(3.85,26.5,3.55));
#27771=CARTESIAN_POINT('',(3.85,26.5,3.55));
#27772=CARTESIAN_POINT('Origin',(3.85,26.5,3.55));
#27773=CARTESIAN_POINT('',(3.85,26.5,3.55));
#27774=CARTESIAN_POINT('Origin',(0.,26.5,0.));
#27775=CARTESIAN_POINT('Origin',(0.,1.,0.));
#27776=CARTESIAN_POINT('Origin',(-9.98087141305093E-16,1.,-8.15));
#27777=CARTESIAN_POINT('Origin',(0.,-3.5,0.));
#27778=CARTESIAN_POINT('',(0.,0.,0.));
#27779=CARTESIAN_POINT('Origin',(0.,7.5,0.));
#27780=CARTESIAN_POINT('',(3.5,7.5,3.75));
#27781=CARTESIAN_POINT('',(3.5,7.5,-3.75));
#27782=CARTESIAN_POINT('',(3.5,7.5,3.75));
#27783=CARTESIAN_POINT('',(-3.5,7.5,-3.75));
#27784=CARTESIAN_POINT('',(-3.5,7.5,-3.75));
#27785=CARTESIAN_POINT('',(-3.5,7.5,3.75));
#27786=CARTESIAN_POINT('',(-3.5,7.5,3.75));
#27787=CARTESIAN_POINT('',(-3.5,7.5,3.75));
#27788=CARTESIAN_POINT('',(-1.13411058466707,7.5,1.43083506494736));
#27789=CARTESIAN_POINT('',(-1.13411058466707,7.5,-2.06916493505264));
#27790=CARTESIAN_POINT('',(-1.13411058466707,7.5,1.43083506494736));
#27791=CARTESIAN_POINT('',(-0.820008020564509,7.5,-2.06916493505264));
#27792=CARTESIAN_POINT('',(-1.13411058466707,7.5,-2.06916493505264));
#27793=CARTESIAN_POINT('',(-0.820008020564509,7.5,-0.633267499155203));
#27794=CARTESIAN_POINT('',(-0.820008020564509,7.5,-2.06916493505264));
#27795=CARTESIAN_POINT('',(0.974863774307286,7.5,-0.633267499155203));
#27796=CARTESIAN_POINT('',(-0.820008020564509,7.5,-0.633267499155203));
#27797=CARTESIAN_POINT('',(0.974863774307286,7.5,-2.06916493505264));
#27798=CARTESIAN_POINT('',(0.974863774307286,7.5,-0.633267499155203));
#27799=CARTESIAN_POINT('',(1.28896633840985,7.5,-2.06916493505264));
#27800=CARTESIAN_POINT('',(0.974863774307286,7.5,-2.06916493505264));
#27801=CARTESIAN_POINT('',(1.28896633840985,7.5,1.43083506494736));
#27802=CARTESIAN_POINT('',(1.28896633840985,7.5,-2.06916493505264));
#27803=CARTESIAN_POINT('',(0.974863774307286,7.5,1.43083506494736));
#27804=CARTESIAN_POINT('',(1.28896633840985,7.5,1.43083506494736));
#27805=CARTESIAN_POINT('',(0.974863774307286,7.5,-0.274293140180844));
#27806=CARTESIAN_POINT('',(0.974863774307286,7.5,1.43083506494736));
#27807=CARTESIAN_POINT('',(-0.820008020564509,7.5,-0.274293140180844));
#27808=CARTESIAN_POINT('',(0.974863774307286,7.5,-0.274293140180844));
#27809=CARTESIAN_POINT('',(-0.820008020564509,7.5,1.43083506494736));
#27810=CARTESIAN_POINT('',(-0.820008020564509,7.5,-0.274293140180844));
#27811=CARTESIAN_POINT('',(-0.820008020564509,7.5,1.43083506494736));
#27812=CARTESIAN_POINT('Origin',(3.5,7.5,3.75));
#27813=CARTESIAN_POINT('',(3.5,0.,3.75));
#27814=CARTESIAN_POINT('',(3.5,0.,-3.75));
#27815=CARTESIAN_POINT('',(3.5,0.,3.75));
#27816=CARTESIAN_POINT('',(3.5,7.5,-3.75));
#27817=CARTESIAN_POINT('',(3.5,7.5,3.75));
#27818=CARTESIAN_POINT('Origin',(-3.5,7.5,-3.75));
#27819=CARTESIAN_POINT('',(-3.5,0.,-3.75));
#27820=CARTESIAN_POINT('',(-3.5,0.,-3.75));
#27821=CARTESIAN_POINT('',(-3.5,7.5,-3.75));
#27822=CARTESIAN_POINT('Origin',(-3.5,7.5,3.75));
#27823=CARTESIAN_POINT('',(-3.5,0.,3.75));
#27824=CARTESIAN_POINT('',(-3.5,0.,3.75));
#27825=CARTESIAN_POINT('',(-3.5,7.5,3.75));
#27826=CARTESIAN_POINT('Origin',(-3.5,7.5,3.75));
#27827=CARTESIAN_POINT('',(-3.5,0.,3.75));
#27828=CARTESIAN_POINT('Origin',(0.,0.,0.));
#27829=CARTESIAN_POINT('',(-1.13411058466707,0.,1.43083506494736));
#27830=CARTESIAN_POINT('',(-1.13411058466707,0.,-2.06916493505264));
#27831=CARTESIAN_POINT('',(-1.13411058466707,0.,1.43083506494736));
#27832=CARTESIAN_POINT('',(-0.820008020564509,0.,1.43083506494736));
#27833=CARTESIAN_POINT('',(-0.820008020564509,0.,1.43083506494736));
#27834=CARTESIAN_POINT('',(-0.820008020564509,0.,-0.274293140180844));
#27835=CARTESIAN_POINT('',(-0.820008020564509,0.,-0.274293140180844));
#27836=CARTESIAN_POINT('',(0.974863774307286,0.,-0.274293140180844));
#27837=CARTESIAN_POINT('',(0.974863774307286,0.,-0.274293140180844));
#27838=CARTESIAN_POINT('',(0.974863774307286,0.,1.43083506494736));
#27839=CARTESIAN_POINT('',(0.974863774307286,0.,1.43083506494736));
#27840=CARTESIAN_POINT('',(1.28896633840985,0.,1.43083506494736));
#27841=CARTESIAN_POINT('',(1.28896633840985,0.,1.43083506494736));
#27842=CARTESIAN_POINT('',(1.28896633840985,0.,-2.06916493505264));
#27843=CARTESIAN_POINT('',(1.28896633840985,0.,-2.06916493505264));
#27844=CARTESIAN_POINT('',(0.974863774307286,0.,-2.06916493505264));
#27845=CARTESIAN_POINT('',(0.974863774307286,0.,-2.06916493505264));
#27846=CARTESIAN_POINT('',(0.974863774307286,0.,-0.633267499155203));
#27847=CARTESIAN_POINT('',(0.974863774307286,0.,-0.633267499155203));
#27848=CARTESIAN_POINT('',(-0.820008020564509,0.,-0.633267499155203));
#27849=CARTESIAN_POINT('',(-0.820008020564509,0.,-0.633267499155203));
#27850=CARTESIAN_POINT('',(-0.820008020564509,0.,-2.06916493505264));
#27851=CARTESIAN_POINT('',(-0.820008020564509,0.,-2.06916493505264));
#27852=CARTESIAN_POINT('',(-1.13411058466707,0.,-2.06916493505264));
#27853=CARTESIAN_POINT('Origin',(-1.13411058466707,7.45,1.43083506494736));
#27854=CARTESIAN_POINT('',(-1.13411058466707,7.45,1.43083506494736));
#27855=CARTESIAN_POINT('',(-1.13411058466707,7.45,1.43083506494736));
#27856=CARTESIAN_POINT('',(-1.13411058466707,7.45,-2.06916493505264));
#27857=CARTESIAN_POINT('',(-1.13411058466707,7.45,1.43083506494736));
#27858=CARTESIAN_POINT('',(-1.13411058466707,7.45,-2.06916493505264));
#27859=CARTESIAN_POINT('Origin',(-1.13411058466707,7.45,-2.06916493505264));
#27860=CARTESIAN_POINT('',(-0.820008020564509,7.45,-2.06916493505264));
#27861=CARTESIAN_POINT('',(-1.13411058466707,7.45,-2.06916493505264));
#27862=CARTESIAN_POINT('',(-0.820008020564509,7.45,-2.06916493505264));
#27863=CARTESIAN_POINT('Origin',(-0.820008020564509,7.45,-2.06916493505264));
#27864=CARTESIAN_POINT('',(-0.820008020564509,7.45,-0.633267499155203));
#27865=CARTESIAN_POINT('',(-0.820008020564509,7.45,-2.06916493505264));
#27866=CARTESIAN_POINT('',(-0.820008020564509,7.45,-0.633267499155203));
#27867=CARTESIAN_POINT('Origin',(-0.820008020564509,7.45,-0.633267499155203));
#27868=CARTESIAN_POINT('',(0.974863774307286,7.45,-0.633267499155203));
#27869=CARTESIAN_POINT('',(-0.820008020564509,7.45,-0.633267499155203));
#27870=CARTESIAN_POINT('',(0.974863774307286,7.45,-0.633267499155203));
#27871=CARTESIAN_POINT('Origin',(0.974863774307286,7.45,-0.633267499155203));
#27872=CARTESIAN_POINT('',(0.974863774307286,7.45,-2.06916493505264));
#27873=CARTESIAN_POINT('',(0.974863774307286,7.45,-0.633267499155203));
#27874=CARTESIAN_POINT('',(0.974863774307286,7.45,-2.06916493505264));
#27875=CARTESIAN_POINT('Origin',(0.974863774307286,7.45,-2.06916493505264));
#27876=CARTESIAN_POINT('',(1.28896633840985,7.45,-2.06916493505264));
#27877=CARTESIAN_POINT('',(0.974863774307286,7.45,-2.06916493505264));
#27878=CARTESIAN_POINT('',(1.28896633840985,7.45,-2.06916493505264));
#27879=CARTESIAN_POINT('Origin',(1.28896633840985,7.45,-2.06916493505264));
#27880=CARTESIAN_POINT('',(1.28896633840985,7.45,1.43083506494736));
#27881=CARTESIAN_POINT('',(1.28896633840985,7.45,-2.06916493505264));
#27882=CARTESIAN_POINT('',(1.28896633840985,7.45,1.43083506494736));
#27883=CARTESIAN_POINT('Origin',(1.28896633840985,7.45,1.43083506494736));
#27884=CARTESIAN_POINT('',(0.974863774307286,7.45,1.43083506494736));
#27885=CARTESIAN_POINT('',(1.28896633840985,7.45,1.43083506494736));
#27886=CARTESIAN_POINT('',(0.974863774307286,7.45,1.43083506494736));
#27887=CARTESIAN_POINT('Origin',(0.974863774307286,7.45,1.43083506494736));
#27888=CARTESIAN_POINT('',(0.974863774307286,7.45,-0.274293140180844));
#27889=CARTESIAN_POINT('',(0.974863774307286,7.45,1.43083506494736));
#27890=CARTESIAN_POINT('',(0.974863774307286,7.45,-0.274293140180844));
#27891=CARTESIAN_POINT('Origin',(0.974863774307286,7.45,-0.274293140180844));
#27892=CARTESIAN_POINT('',(-0.820008020564509,7.45,-0.274293140180844));
#27893=CARTESIAN_POINT('',(0.974863774307286,7.45,-0.274293140180844));
#27894=CARTESIAN_POINT('',(-0.820008020564509,7.45,-0.274293140180844));
#27895=CARTESIAN_POINT('Origin',(-0.820008020564509,7.45,-0.274293140180844));
#27896=CARTESIAN_POINT('',(-0.820008020564509,7.45,1.43083506494736));
#27897=CARTESIAN_POINT('',(-0.820008020564509,7.45,-0.274293140180844));
#27898=CARTESIAN_POINT('',(-0.820008020564509,7.45,1.43083506494736));
#27899=CARTESIAN_POINT('Origin',(-0.820008020564509,7.45,1.43083506494736));
#27900=CARTESIAN_POINT('',(-0.820008020564509,7.45,1.43083506494736));
#27901=CARTESIAN_POINT('Origin',(0.,7.45,0.));
#27902=CARTESIAN_POINT('Origin',(-1.13411058466707,0.05,1.43083506494736));
#27903=CARTESIAN_POINT('',(-1.13411058466707,0.05,-2.06916493505264));
#27904=CARTESIAN_POINT('',(-1.13411058466707,0.05,-2.06916493505264));
#27905=CARTESIAN_POINT('',(-1.13411058466707,0.05,1.43083506494736));
#27906=CARTESIAN_POINT('',(-1.13411058466707,0.05,1.43083506494736));
#27907=CARTESIAN_POINT('',(-1.13411058466707,0.05,1.43083506494736));
#27908=CARTESIAN_POINT('Origin',(-0.820008020564509,0.05,1.43083506494736));
#27909=CARTESIAN_POINT('',(-0.820008020564509,0.05,1.43083506494736));
#27910=CARTESIAN_POINT('',(-0.820008020564509,0.05,1.43083506494736));
#27911=CARTESIAN_POINT('',(-0.820008020564509,0.05,1.43083506494736));
#27912=CARTESIAN_POINT('Origin',(-0.820008020564509,0.05,-0.274293140180844));
#27913=CARTESIAN_POINT('',(-0.820008020564509,0.05,-0.274293140180844));
#27914=CARTESIAN_POINT('',(-0.820008020564509,0.05,-0.274293140180844));
#27915=CARTESIAN_POINT('',(-0.820008020564509,0.05,-0.274293140180844));
#27916=CARTESIAN_POINT('Origin',(0.974863774307286,0.05,-0.274293140180844));
#27917=CARTESIAN_POINT('',(0.974863774307286,0.05,-0.274293140180844));
#27918=CARTESIAN_POINT('',(0.974863774307286,0.05,-0.274293140180844));
#27919=CARTESIAN_POINT('',(0.974863774307286,0.05,-0.274293140180844));
#27920=CARTESIAN_POINT('Origin',(0.974863774307286,0.05,1.43083506494736));
#27921=CARTESIAN_POINT('',(0.974863774307286,0.05,1.43083506494736));
#27922=CARTESIAN_POINT('',(0.974863774307286,0.05,1.43083506494736));
#27923=CARTESIAN_POINT('',(0.974863774307286,0.05,1.43083506494736));
#27924=CARTESIAN_POINT('Origin',(1.28896633840985,0.05,1.43083506494736));
#27925=CARTESIAN_POINT('',(1.28896633840985,0.05,1.43083506494736));
#27926=CARTESIAN_POINT('',(1.28896633840985,0.05,1.43083506494736));
#27927=CARTESIAN_POINT('',(1.28896633840985,0.05,1.43083506494736));
#27928=CARTESIAN_POINT('Origin',(1.28896633840985,0.05,-2.06916493505264));
#27929=CARTESIAN_POINT('',(1.28896633840985,0.05,-2.06916493505264));
#27930=CARTESIAN_POINT('',(1.28896633840985,0.05,-2.06916493505264));
#27931=CARTESIAN_POINT('',(1.28896633840985,0.05,-2.06916493505264));
#27932=CARTESIAN_POINT('Origin',(0.974863774307286,0.05,-2.06916493505264));
#27933=CARTESIAN_POINT('',(0.974863774307286,0.05,-2.06916493505264));
#27934=CARTESIAN_POINT('',(0.974863774307286,0.05,-2.06916493505264));
#27935=CARTESIAN_POINT('',(0.974863774307286,0.05,-2.06916493505264));
#27936=CARTESIAN_POINT('Origin',(0.974863774307286,0.05,-0.633267499155203));
#27937=CARTESIAN_POINT('',(0.974863774307286,0.05,-0.633267499155203));
#27938=CARTESIAN_POINT('',(0.974863774307286,0.05,-0.633267499155203));
#27939=CARTESIAN_POINT('',(0.974863774307286,0.05,-0.633267499155203));
#27940=CARTESIAN_POINT('Origin',(-0.820008020564509,0.05,-0.633267499155203));
#27941=CARTESIAN_POINT('',(-0.820008020564509,0.05,-0.633267499155203));
#27942=CARTESIAN_POINT('',(-0.820008020564509,0.05,-0.633267499155203));
#27943=CARTESIAN_POINT('',(-0.820008020564509,0.05,-0.633267499155203));
#27944=CARTESIAN_POINT('Origin',(-0.820008020564509,0.05,-2.06916493505264));
#27945=CARTESIAN_POINT('',(-0.820008020564509,0.05,-2.06916493505264));
#27946=CARTESIAN_POINT('',(-0.820008020564509,0.05,-2.06916493505264));
#27947=CARTESIAN_POINT('',(-0.820008020564509,0.05,-2.06916493505264));
#27948=CARTESIAN_POINT('Origin',(-1.13411058466707,0.05,-2.06916493505264));
#27949=CARTESIAN_POINT('',(-1.13411058466707,0.05,-2.06916493505264));
#27950=CARTESIAN_POINT('Origin',(0.,0.05,0.));
#27951=CARTESIAN_POINT('',(0.,0.,0.));
#27952=CARTESIAN_POINT('Origin',(0.,0.,0.));
#27953=CARTESIAN_POINT('',(-10.2,0.,-4.59242549680259E-17));
#27954=CARTESIAN_POINT('Origin',(-10.575,0.,0.));
#27955=CARTESIAN_POINT('',(-10.0450390807245,-1.77121141220256,-4.59242549680259E-17));
#27956=CARTESIAN_POINT('Origin',(0.,0.,-4.59242549680259E-17));
#27957=CARTESIAN_POINT('Origin',(-10.4143419881041,-1.83632947882765,0.));
#27958=CARTESIAN_POINT('Origin',(-10.4143419881041,-1.83632947882765,0.));
#27959=CARTESIAN_POINT('Origin',(-10.575,0.,0.));
#27960=CARTESIAN_POINT('',(0.,0.,0.));
#27961=CARTESIAN_POINT('Origin',(0.,1.90000000000001,-9.86076131526265E-29));
#27962=CARTESIAN_POINT('',(1.10261122559919E-28,0.,8.925));
#27963=CARTESIAN_POINT('Origin',(0.,0.,0.));
#27964=CARTESIAN_POINT('',(1.10261122559919E-28,1.90000000000001,8.925));
#27965=CARTESIAN_POINT('',(-1.0929972682389E-15,1.90000000000001,8.925));
#27966=CARTESIAN_POINT('Origin',(0.,1.90000000000001,-9.86076131526265E-29));
#27967=CARTESIAN_POINT('Origin',(0.,1.90000000000001,-9.86076131526265E-29));
#27968=CARTESIAN_POINT('Origin',(0.,0.,0.));
#27969=CARTESIAN_POINT('',(0.,0.,0.));
#27970=CARTESIAN_POINT('Origin',(0.,13.,0.));
#27971=CARTESIAN_POINT('',(0.,13.,9.15));
#27972=CARTESIAN_POINT('Origin',(0.,13.,0.));
#27973=CARTESIAN_POINT('',(0.,13.,7.25));
#27974=CARTESIAN_POINT('Origin',(0.,13.,0.));
#27975=CARTESIAN_POINT('Origin',(0.,0.,0.));
#27976=CARTESIAN_POINT('',(0.,0.,9.15));
#27977=CARTESIAN_POINT('Origin',(0.,0.,0.));
#27978=CARTESIAN_POINT('',(0.,0.,7.25));
#27979=CARTESIAN_POINT('Origin',(0.,0.,0.));
#27980=CARTESIAN_POINT('Origin',(0.,13.,0.));
#27981=CARTESIAN_POINT('',(-1.12055182121983E-15,13.,9.15));
#27982=CARTESIAN_POINT('Origin',(0.,13.,0.));
#27983=CARTESIAN_POINT('',(-8.87868929381831E-16,13.,7.25));
#27984=CARTESIAN_POINT('',(0.,0.,0.));
#27985=CARTESIAN_POINT('',(0.,0.,0.));
#27986=CARTESIAN_POINT('',(-8.91814653729712E-15,-1.18560712151112E-12,
-55.4999999999998));
#27987=CARTESIAN_POINT('',(-3.16413562017393E-15,-8.11769411281129E-14,
23.2500000000002));
#27988=CARTESIAN_POINT('',(7.5190140746845E-15,-1.25572341693254E-13,25.1500000000002));
#27989=CARTESIAN_POINT('',(6.58572362436991E-15,-4.54488320527988E-13,117.05));
#27990=CARTESIAN_POINT('',(-1.08166107364382E-14,-5.23452079948658E-13,
143.55));
#27991=CARTESIAN_POINT('',(0.,0.,76.2));
#27992=CARTESIAN_POINT('',(-4.90956723382788E-17,-1.19714133913152E-13,
33.7864015016378));
#27993=CARTESIAN_POINT('',(5.32118521506748E-15,-4.28767844901084E-13,115.15));
#27994=CARTESIAN_POINT('',(2.54961294583579E-30,-1.38507551587588E-13,39.4864015016377));
#27995=CARTESIAN_POINT('',(1.26940635170459E-26,-1.25239922500056E-13,35.6864015016377));
#27996=CARTESIAN_POINT('',(4.66540068069163E-27,-1.3187373704399E-13,37.5864015016377));
#27997=CARTESIAN_POINT('',(2.12432532903342E-17,-7.37159978726724E-14,20.7864015016377));
#27998=CARTESIAN_POINT('',(0.,0.,0.));
#27999=CARTESIAN_POINT('Origin',(0.,0.,0.));
#28000=CARTESIAN_POINT('',(-3.67394039744206E-16,2.1,3.));
#28001=CARTESIAN_POINT('Origin',(0.,2.1,0.));
#28002=CARTESIAN_POINT('',(-3.67394039744206E-16,25.,3.));
#28003=CARTESIAN_POINT('',(-3.67394039744206E-16,0.,3.));
#28004=CARTESIAN_POINT('Origin',(0.,25.,0.));
#28005=CARTESIAN_POINT('Origin',(-3.75,25.,0.));
#28006=CARTESIAN_POINT('',(-4.59242549680257E-16,25.,3.75));
#28007=CARTESIAN_POINT('Origin',(0.,25.,0.));
#28008=CARTESIAN_POINT('Origin',(0.,0.,0.));
#28009=CARTESIAN_POINT('',(-4.59242549680257E-16,26.,3.75));
#28010=CARTESIAN_POINT('',(-4.59242549680257E-16,0.,3.75));
#28011=CARTESIAN_POINT('Origin',(0.,26.,0.));
#28012=CARTESIAN_POINT('Origin',(0.,26.,0.));
#28013=CARTESIAN_POINT('Origin',(-3.,1.1,0.));
#28014=CARTESIAN_POINT('',(-3.67394039744206E-16,1.1,3.));
#28015=CARTESIAN_POINT('Origin',(0.,1.1,0.));
#28016=CARTESIAN_POINT('',(-2.93915231795365E-16,1.1,2.4));
#28017=CARTESIAN_POINT('Origin',(0.,1.1,0.));
#28018=CARTESIAN_POINT('Origin',(0.,0.,0.));
#28019=CARTESIAN_POINT('',(-2.93915231795365E-16,2.1,2.4));
#28020=CARTESIAN_POINT('',(-2.93915231795365E-16,0.,2.4));
#28021=CARTESIAN_POINT('Origin',(0.,2.1,0.));
#28022=CARTESIAN_POINT('Origin',(-3.,2.1,0.));
#28023=CARTESIAN_POINT('Origin',(0.,0.,0.));
#28024=CARTESIAN_POINT('',(-3.67394039744206E-16,0.,3.));
#28025=CARTESIAN_POINT('Origin',(0.,0.,0.));
#28026=CARTESIAN_POINT('Origin',(0.,0.,0.));
#28027=CARTESIAN_POINT('',(-3.67394039744206E-16,0.,3.));
#28028=CARTESIAN_POINT('',(0.,0.,0.));
#28029=CARTESIAN_POINT('',(0.,0.,0.));
#28030=CARTESIAN_POINT('Origin',(0.,0.,0.));
#28031=CARTESIAN_POINT('',(-3.38063404204883,17.1703614834907,5.26598123633362E-16));
#28032=CARTESIAN_POINT('',(-7.35749486474657,15.8782010730192,5.26598123633362E-16));
#28033=CARTESIAN_POINT('Origin',(0.,0.,5.26598123633362E-16));
#28034=CARTESIAN_POINT('',(-7.75098709974896,15.6898756840048,0.134720657333156));
#28035=CARTESIAN_POINT('Ctrl Pts',(-7.35749486474656,15.8782010730192,4.02239005992122E-16));
#28036=CARTESIAN_POINT('Ctrl Pts',(-7.40654917656635,15.8554707369032,-1.1304709011049E-17));
#28037=CARTESIAN_POINT('Ctrl Pts',(-7.45547662735319,15.8325185186142,0.0057118776195191));
#28038=CARTESIAN_POINT('Ctrl Pts',(-7.58311255681024,15.771945196048,0.0353494158279855));
#28039=CARTESIAN_POINT('Ctrl Pts',(-7.66048059708591,15.7344445945251,0.0693026530250561));
#28040=CARTESIAN_POINT('Ctrl Pts',(-7.73596042367391,15.6972924318009,0.123164970119313));
#28041=CARTESIAN_POINT('Ctrl Pts',(-7.74353659553706,15.6935563226023,0.12884558346146));
#28042=CARTESIAN_POINT('Ctrl Pts',(-7.75098709974896,15.6898756840048,0.134720657333156));
#28043=CARTESIAN_POINT('',(-7.75098748126848,15.6898754955296,98.476464169983));
#28044=CARTESIAN_POINT('',(-7.75098709974896,15.6898756840048,0.));
#28045=CARTESIAN_POINT('',(-7.62166407822416,15.7531022199328,98.5000002325512));
#28046=CARTESIAN_POINT('Ctrl Pts',(-7.75098827006065,15.6898751058567,98.4764666117908));
#28047=CARTESIAN_POINT('Ctrl Pts',(-7.73036519553247,15.7000631543709,98.4847544570797));
#28048=CARTESIAN_POINT('Ctrl Pts',(-7.70899812928367,15.7105675084655,98.4906432907328));
#28049=CARTESIAN_POINT('Ctrl Pts',(-7.6656344940948,15.7317713310211,98.4982621653015));
#28050=CARTESIAN_POINT('Ctrl Pts',(-7.64364124698384,15.7424694536167,98.5000001531237));
#28051=CARTESIAN_POINT('Ctrl Pts',(-7.62166492311257,15.7531020373701,98.5000000867633));
#28052=CARTESIAN_POINT('',(-3.09338542091479,17.2244295086968,98.5000006225421));
#28053=CARTESIAN_POINT('Origin',(0.,0.,98.5));
#28054=CARTESIAN_POINT('',(-2.95159725048241,17.2492919759318,98.4764616066469));
#28055=CARTESIAN_POINT('Ctrl Pts',(-3.09338528775832,17.2244293798512,98.5000011593602));
#28056=CARTESIAN_POINT('Ctrl Pts',(-3.06935680199578,17.228744725382,98.5000018789964));
#28057=CARTESIAN_POINT('Ctrl Pts',(-3.04527498726421,17.2330171964727,98.4982647459743));
#28058=CARTESIAN_POINT('Ctrl Pts',(-2.99772878170085,17.241351622266,98.4906474053966));
#28059=CARTESIAN_POINT('Ctrl Pts',(-2.97426775127845,17.2454127370105,98.4847593539947));
#28060=CARTESIAN_POINT('Ctrl Pts',(-2.95159454990789,17.249292438038,98.4764721130873));
#28061=CARTESIAN_POINT('',(-2.95159725048241,17.2492919759318,0.134720657333159));
#28062=CARTESIAN_POINT('',(-2.95159725048241,17.2492919759318,0.));
#28063=CARTESIAN_POINT('Ctrl Pts',(-2.95159725048241,17.2492919759318,0.134720657333162));
#28064=CARTESIAN_POINT('Ctrl Pts',(-3.01054883678071,17.2392045276891,0.0924371122250883));
#28065=CARTESIAN_POINT('Ctrl Pts',(-3.07862853003574,17.2272341593699,0.0586496504523806));
#28066=CARTESIAN_POINT('Ctrl Pts',(-3.22585327793649,17.2002767814783,0.0120815387590075));
#28067=CARTESIAN_POINT('Ctrl Pts',(-3.3034974264849,17.1855487390831,4.12448671408897E-16));
#28068=CARTESIAN_POINT('Ctrl Pts',(-3.38063404204883,17.1703614834907,4.16333634234434E-16));
#28069=CARTESIAN_POINT('Origin',(0.,0.,0.));
#28070=CARTESIAN_POINT('',(7.7509870154707,15.6898756108788,98.4764611650906));
#28071=CARTESIAN_POINT('',(7.75098709974897,15.6898756840048,0.13472065733317));
#28072=CARTESIAN_POINT('',(7.75098709974897,15.6898756840048,0.));
#28073=CARTESIAN_POINT('',(7.35749486474656,15.8782010730192,5.26598123633362E-16));
#28074=CARTESIAN_POINT('Ctrl Pts',(7.75098709974897,15.6898756840048,0.134720657333169));
#28075=CARTESIAN_POINT('Ctrl Pts',(7.697365011278,15.716365639972,0.092437112225102));
#28076=CARTESIAN_POINT('Ctrl Pts',(7.6352513765003,15.7466976482487,0.0586496504523873));
#28077=CARTESIAN_POINT('Ctrl Pts',(7.50029890429084,15.8114252069992,0.0120815387590058));
#28078=CARTESIAN_POINT('Ctrl Pts',(7.42882654248636,15.8451480558511,-2.91946290751094E-16));
#28079=CARTESIAN_POINT('Ctrl Pts',(7.35749486474656,15.8782010730192,4.16333634234434E-16));
#28080=CARTESIAN_POINT('',(3.38063404204883,17.1703614834907,5.26598123633362E-16));
#28081=CARTESIAN_POINT('Origin',(0.,0.,5.26598123633362E-16));
#28082=CARTESIAN_POINT('',(2.95159725048241,17.2492919759318,0.134720657333159));
#28083=CARTESIAN_POINT('Ctrl Pts',(3.38063404204883,17.1703614834907,3.78386558197441E-16));
#28084=CARTESIAN_POINT('Ctrl Pts',(3.32758771379059,17.180805656334,3.54366411019119E-16));
#28085=CARTESIAN_POINT('Ctrl Pts',(3.27451359919498,17.1909957556844,0.00571187761951955));
#28086=CARTESIAN_POINT('Ctrl Pts',(3.13564985748462,17.2170134253201,0.0353494158279847));
#28087=CARTESIAN_POINT('Ctrl Pts',(3.05101549755283,17.2321505944616,0.0693026530250554));
#28088=CARTESIAN_POINT('Ctrl Pts',(2.96811354177061,17.2464597923539,0.123164970119314));
#28089=CARTESIAN_POINT('Ctrl Pts',(2.95978826009315,17.2478903786094,0.128845583461463));
#28090=CARTESIAN_POINT('Ctrl Pts',(2.95159725048241,17.2492919759318,0.134720657333162));
#28091=CARTESIAN_POINT('',(2.95159683426415,17.2492920471526,98.4764641502857));
#28092=CARTESIAN_POINT('',(2.95159725048241,17.2492919759318,0.));
#28093=CARTESIAN_POINT('',(3.09338455449675,17.2244295302922,98.5000000582798));
#28094=CARTESIAN_POINT('Ctrl Pts',(2.95159597373243,17.2492921944017,98.4764665733303));
#28095=CARTESIAN_POINT('Ctrl Pts',(2.97426877032574,17.245412560711,98.4847544660921));
#28096=CARTESIAN_POINT('Ctrl Pts',(2.99772938956493,17.2413515161254,98.4906433246677));
#28097=CARTESIAN_POINT('Ctrl Pts',(3.04527460155141,17.2330172636463,98.4982622140882));
#28098=CARTESIAN_POINT('Ctrl Pts',(3.06935553227654,17.2287449523539,98.5000001907974));
#28099=CARTESIAN_POINT('Ctrl Pts',(3.09338455123434,17.2244295121256,98.5000001151055));
#28100=CARTESIAN_POINT('',(7.62166294207788,15.7531030650529,98.5000002711098));
#28101=CARTESIAN_POINT('Origin',(0.,0.,98.5));
#28102=CARTESIAN_POINT('Ctrl Pts',(7.62166291493897,15.7531030089644,98.5000005001312));
#28103=CARTESIAN_POINT('Ctrl Pts',(7.6436435511221,15.7424683422865,98.5000007104308));
#28104=CARTESIAN_POINT('Ctrl Pts',(7.66563431697673,15.7317714169945,98.4982623363922));
#28105=CARTESIAN_POINT('Ctrl Pts',(7.70900073858223,15.7105662332998,98.4906410122901));
#28106=CARTESIAN_POINT('Ctrl Pts',(7.73036164225094,15.7000649076559,98.4847522013256));
#28107=CARTESIAN_POINT('Ctrl Pts',(7.7509869987881,15.6898757338807,98.4764609724326));
#28108=CARTESIAN_POINT('Origin',(0.,0.,0.));
#28109=CARTESIAN_POINT('',(15.4929577055454,8.13746014975801,98.4764611351391));
#28110=CARTESIAN_POINT('',(15.4929578242382,8.13746016004849,0.134720657333155));
#28111=CARTESIAN_POINT('',(15.4929578242382,8.13746016004849,0.));
#28112=CARTESIAN_POINT('',(15.2853108052616,8.52110753285942,5.26598123633362E-16));
#28113=CARTESIAN_POINT('Ctrl Pts',(15.4929578242382,8.13746016004849,0.134720657333156));
#28114=CARTESIAN_POINT('Ctrl Pts',(15.4651470488427,8.19040925740651,0.0924371122251327));
#28115=CARTESIAN_POINT('Ctrl Pts',(15.4327247698627,8.25145784606448,0.0586496504524068));
#28116=CARTESIAN_POINT('Ctrl Pts',(15.3615918308627,8.38314661402319,0.0120815387590046));
#28117=CARTESIAN_POINT('Ctrl Pts',(15.3235912687552,8.45243937205836,-8.0627802103072E-17));
#28118=CARTESIAN_POINT('Ctrl Pts',(15.2853108052616,8.52110753285941,4.16333634234434E-16));
#28119=CARTESIAN_POINT('',(12.8274756483065,11.9040274063908,5.26598123633362E-16));
#28120=CARTESIAN_POINT('Origin',(0.,0.,5.26598123633362E-16));
#28121=CARTESIAN_POINT('',(12.5267717721302,12.2200650149237,0.134720657333169));
#28122=CARTESIAN_POINT('Ctrl Pts',(12.8274756483065,11.9040274063908,4.38017677684144E-16));
#28123=CARTESIAN_POINT('Ctrl Pts',(12.7906991980261,11.9436567691517,-2.13930726438973E-16));
#28124=CARTESIAN_POINT('Ctrl Pts',(12.7537509274744,11.9830969145383,0.00571187761951889));
#28125=CARTESIAN_POINT('Ctrl Pts',(12.6567006030391,12.0857677108831,0.0353494158279851));
#28126=CARTESIAN_POINT('Ctrl Pts',(12.597127372329,12.1477607665704,0.0693026530250562));
#28127=CARTESIAN_POINT('Ctrl Pts',(12.5384690167276,12.2080656978362,0.123164970119317));
#28128=CARTESIAN_POINT('Ctrl Pts',(12.5325745998707,12.2141165442201,0.128845583461466));
#28129=CARTESIAN_POINT('Ctrl Pts',(12.5267717721302,12.2200650149237,0.134720657333167));
#28130=CARTESIAN_POINT('',(12.5267714753738,12.2200653191283,98.4764641666045));
#28131=CARTESIAN_POINT('',(12.5267717721302,12.2200650149237,0.));
#28132=CARTESIAN_POINT('',(12.6268663170878,12.1166104030896,98.5000000583843));
#28133=CARTESIAN_POINT('Ctrl Pts',(12.5267708618295,12.2200659480716,98.4764666051942));
#28134=CARTESIAN_POINT('Ctrl Pts',(12.5428331499379,12.2036005211659,98.4847544881405));
#28135=CARTESIAN_POINT('Ctrl Pts',(12.5594261690095,12.1865252595175,98.4906433390831));
#28136=CARTESIAN_POINT('Ctrl Pts',(12.5929923076291,12.1518363282392,98.4982622190212));
#28137=CARTESIAN_POINT('Ctrl Pts',(12.6099629957874,12.1342255319368,98.5000001912344));
#28138=CARTESIAN_POINT('Ctrl Pts',(12.6268663036908,12.1166103902337,98.500000115428));
#28139=CARTESIAN_POINT('',(15.4254964602665,8.26462701674586,98.5000002246578));
#28140=CARTESIAN_POINT('Origin',(0.,0.,98.5));
#28141=CARTESIAN_POINT('Ctrl Pts',(15.4254964408324,8.26462700633656,98.5000005203777));
#28142=CARTESIAN_POINT('Ctrl Pts',(15.4370282602941,8.24310346511366,98.5000007416219));
#28143=CARTESIAN_POINT('Ctrl Pts',(15.4485316552151,8.22152364814352,98.4982623777968));
#28144=CARTESIAN_POINT('Ctrl Pts',(15.471151745739,8.17887812715057,98.4906410339749));
#28145=CARTESIAN_POINT('Ctrl Pts',(15.4822605547264,8.15782675347633,98.4847521990831));
#28146=CARTESIAN_POINT('Ctrl Pts',(15.4929577683353,8.13746026648231,98.4764609294304));
#28147=CARTESIAN_POINT('Origin',(0.,0.,0.));
#28148=CARTESIAN_POINT('',(17.3171451173558,-2.52318944679936,98.4764669873976));
#28149=CARTESIAN_POINT('',(17.3171452461371,-2.52318856294819,0.134720657333157));
#28150=CARTESIAN_POINT('',(17.3171452461371,-2.52318856294819,0.));
#28151=CARTESIAN_POINT('',(17.3746575467727,-2.0907594630599,5.26598123633362E-16));
#28152=CARTESIAN_POINT('Ctrl Pts',(17.3171452461371,-2.52318856294818,0.134720657333159));
#28153=CARTESIAN_POINT('Ctrl Pts',(17.3257685547646,-2.46400507971643,0.0924371122251101));
#28154=CARTESIAN_POINT('Ctrl Pts',(17.3354218401598,-2.3955583965793,0.0586496504523934));
#28155=CARTESIAN_POINT('Ctrl Pts',(17.3552787993477,-2.24720905283605,0.012081538759007));
#28156=CARTESIAN_POINT('Ctrl Pts',(17.3652649600707,-2.1688138640129,4.12448671408897E-16));
#28157=CARTESIAN_POINT('Ctrl Pts',(17.3746575467727,-2.0907594630599,4.16333634234434E-16));
#28158=CARTESIAN_POINT('',(17.3746575467727,2.09075946305989,5.26598123633362E-16));
#28159=CARTESIAN_POINT('Origin',(0.,0.,5.26598123633362E-16));
#28160=CARTESIAN_POINT('',(17.3171452461371,2.52318856294818,0.134720657333156));
#28161=CARTESIAN_POINT('Ctrl Pts',(17.3746575467727,2.09075946305989,3.50197301712818E-16));
#28162=CARTESIAN_POINT('Ctrl Pts',(17.3681983284916,2.14443694611619,-1.60626590021751E-17));
#28163=CARTESIAN_POINT('Ctrl Pts',(17.3614888855091,2.19806234252259,0.00571187761951884));
#28164=CARTESIAN_POINT('Ctrl Pts',(17.3433219036639,2.33816951102481,0.0353494158279827));
#28165=CARTESIAN_POINT('Ctrl Pts',(17.3315647514872,2.42333921305185,0.069302653025052));
#28166=CARTESIAN_POINT('Ctrl Pts',(17.3195554941821,2.50660544363676,0.123164970119312));
#28167=CARTESIAN_POINT('Ctrl Pts',(17.3183434090412,2.51496533249098,0.12884558346146));
#28168=CARTESIAN_POINT('Ctrl Pts',(17.3171452461371,2.52318856294818,0.134720657333157));
#28169=CARTESIAN_POINT('',(17.3171451847825,2.52318898403686,98.476464169983));
#28170=CARTESIAN_POINT('',(17.3171452461371,2.52318856294818,0.));
#28171=CARTESIAN_POINT('',(17.3373142437191,2.38065698652278,98.5000002325512));
#28172=CARTESIAN_POINT('Ctrl Pts',(17.3171450579317,2.52318985463833,98.4764666117908));
#28173=CARTESIAN_POINT('Ctrl Pts',(17.3204615873541,2.50042786509176,98.4847544570796));
#28174=CARTESIAN_POINT('Ctrl Pts',(17.3238490351745,2.47686055357144,98.4906432907328));
#28175=CARTESIAN_POINT('Ctrl Pts',(17.3306149685751,2.42906694423961,98.4982621653014));
#28176=CARTESIAN_POINT('Ctrl Pts',(17.3339932006629,2.40484422157029,98.5000001531237));
#28177=CARTESIAN_POINT('Ctrl Pts',(17.3373143311766,2.38065784647434,98.5000000867633));
#28178=CARTESIAN_POINT('',(17.5,-2.14313189850787E-15,98.5));
#28179=CARTESIAN_POINT('Origin',(0.,0.,98.5));
#28180=CARTESIAN_POINT('',(17.337314588927,-2.38065707462705,98.5000006225421));
#28181=CARTESIAN_POINT('Origin',(0.,0.,98.5));
#28182=CARTESIAN_POINT('Ctrl Pts',(17.3373144252399,-2.3806571614509,98.5000011593602));
#28183=CARTESIAN_POINT('Ctrl Pts',(17.3339933522773,-2.40484312451782,98.5000018789964));
#28184=CARTESIAN_POINT('Ctrl Pts',(17.3306150237414,-2.42906655751746,98.4982647459742));
#28185=CARTESIAN_POINT('Ctrl Pts',(17.3238489481645,-2.47686116535237,98.4906474053964));
#28186=CARTESIAN_POINT('Ctrl Pts',(17.3204614406997,-2.50042888468657,98.4847593539944));
#28187=CARTESIAN_POINT('Ctrl Pts',(17.3171448511027,-2.52319127414576,98.476472113087));
#28188=CARTESIAN_POINT('Origin',(0.,0.,0.));
#28189=CARTESIAN_POINT('',(12.8274756483065,-11.9040274063908,5.26598123633362E-16));
#28190=CARTESIAN_POINT('',(15.2853108052616,-8.52110753285942,5.26598123633362E-16));
#28191=CARTESIAN_POINT('Origin',(0.,0.,5.26598123633362E-16));
#28192=CARTESIAN_POINT('',(15.4929578242382,-8.13746016004849,0.134720657333159));
#28193=CARTESIAN_POINT('Ctrl Pts',(15.2853108052616,-8.52110753285942,5.64869331864948E-16));
#28194=CARTESIAN_POINT('Ctrl Pts',(15.3116360208225,-8.47388490360466,5.23827033142938E-16));
#28195=CARTESIAN_POINT('Ctrl Pts',(15.3377281845829,-8.42655733494556,0.00571187761951928));
#28196=CARTESIAN_POINT('Ctrl Pts',(15.4053837149197,-8.30252997058624,0.0353494158279845));
#28197=CARTESIAN_POINT('Ctrl Pts',(15.4459334737969,-8.22671555358209,0.0693026530250558));
#28198=CARTESIAN_POINT('Ctrl Pts',(15.485160442899,-8.15229289364641,0.123164970119313));
#28199=CARTESIAN_POINT('Ctrl Pts',(15.4890936648008,-8.14481715572195,0.128845583461463));
#28200=CARTESIAN_POINT('Ctrl Pts',(15.4929578242382,-8.13746016004849,0.13472065733316));
#28201=CARTESIAN_POINT('',(15.4929580205917,-8.13745978620985,98.4764641502857));
#28202=CARTESIAN_POINT('',(15.4929578242382,-8.13746016004849,0.));
#28203=CARTESIAN_POINT('',(15.4254975467744,-8.26462498123526,98.5000000582797));
#28204=CARTESIAN_POINT('Ctrl Pts',(15.4929584265528,-8.137459013298,98.4764665733302));
#28205=CARTESIAN_POINT('Ctrl Pts',(15.4822623961932,-8.15782325149815,98.4847544660919));
#28206=CARTESIAN_POINT('Ctrl Pts',(15.4711503832338,-8.17888069450974,98.4906433246675));
#28207=CARTESIAN_POINT('Ctrl Pts',(15.4485317595999,-8.22152345253711,98.4982622140881));
#28208=CARTESIAN_POINT('Ctrl Pts',(15.4370271332713,-8.24310556182698,98.5000001907974));
#28209=CARTESIAN_POINT('Ctrl Pts',(15.4254975305051,-8.26462497251875,98.5000001151055));
#28210=CARTESIAN_POINT('',(12.626867931918,-12.1166087252795,98.5000002246578));
#28211=CARTESIAN_POINT('Origin',(0.,0.,98.5));
#28212=CARTESIAN_POINT('',(12.5267717256653,-12.22006490522,98.476461135139));
#28213=CARTESIAN_POINT('Ctrl Pts',(12.6268679160127,-12.1166087100132,98.5000005203778));
#28214=CARTESIAN_POINT('Ctrl Pts',(12.6099613400687,-12.134227262074,98.5000007416219));
#28215=CARTESIAN_POINT('Ctrl Pts',(12.5929924590424,-12.1518361709524,98.4982623777968));
#28216=CARTESIAN_POINT('Ctrl Pts',(12.5594241507975,-12.1865273461652,98.4906410339749));
#28217=CARTESIAN_POINT('Ctrl Pts',(12.5428359154519,-12.2035976835612,98.484752199083));
#28218=CARTESIAN_POINT('Ctrl Pts',(12.5267718560799,-12.220064928867,98.4764609294303));
#28219=CARTESIAN_POINT('',(12.5267717721302,-12.2200650149237,0.134720657333167));
#28220=CARTESIAN_POINT('',(12.5267717721302,-12.2200650149237,0.));
#28221=CARTESIAN_POINT('Ctrl Pts',(12.5267717721302,-12.2200650149237,0.134720657333168));
#28222=CARTESIAN_POINT('Ctrl Pts',(12.5685353539806,-12.1772532248401,0.0924371122250518));
#28223=CARTESIAN_POINT('Ctrl Pts',(12.6165769768333,-12.127552753765,0.0586496504523597));
#28224=CARTESIAN_POINT('Ctrl Pts',(12.7198391507123,-12.0192072413384,0.0120815387590086));
#28225=CARTESIAN_POINT('Ctrl Pts',(12.7739976602867,-11.9616539193032,-7.14583268047246E-16));
#28226=CARTESIAN_POINT('Ctrl Pts',(12.8274756483065,-11.9040274063908,4.16333634234434E-16));
#28227=CARTESIAN_POINT('Origin',(0.,0.,0.));
#28228=CARTESIAN_POINT('',(2.95159637009437,-17.2492921265785,98.4764669873977));
#28229=CARTESIAN_POINT('',(2.95159725048241,-17.2492919759318,0.134720657333156));
#28230=CARTESIAN_POINT('',(2.95159725048241,-17.2492919759318,0.));
#28231=CARTESIAN_POINT('',(3.38063404204883,-17.1703614834907,5.26598123633362E-16));
#28232=CARTESIAN_POINT('Ctrl Pts',(2.95159725048241,-17.2492919759318,0.134720657333158));
#28233=CARTESIAN_POINT('Ctrl Pts',(3.01054883678064,-17.2392045276891,0.092437112225137));
#28234=CARTESIAN_POINT('Ctrl Pts',(3.07862853003564,-17.2272341593699,0.0586496504524089));
#28235=CARTESIAN_POINT('Ctrl Pts',(3.22585327793649,-17.2002767814783,0.0120815387590052));
#28236=CARTESIAN_POINT('Ctrl Pts',(3.3034974264849,-17.1855487390831,2.01130182760907E-16));
#28237=CARTESIAN_POINT('Ctrl Pts',(3.38063404204882,-17.1703614834907,4.16333634234434E-16));
#28238=CARTESIAN_POINT('',(7.35749486474657,-15.8782010730192,5.26598123633362E-16));
#28239=CARTESIAN_POINT('Origin',(0.,0.,5.26598123633362E-16));
#28240=CARTESIAN_POINT('',(7.75098709974897,-15.6898756840048,0.134720657333169));
#28241=CARTESIAN_POINT('Ctrl Pts',(7.35749486474656,-15.8782010730192,5.13911829758129E-16));
#28242=CARTESIAN_POINT('Ctrl Pts',(7.40654917656635,-15.8554707369032,-9.57648980318245E-17));
#28243=CARTESIAN_POINT('Ctrl Pts',(7.45547662735319,-15.8325185186142,0.00571187761951924));
#28244=CARTESIAN_POINT('Ctrl Pts',(7.58311255681024,-15.771945196048,0.0353494158279854));
#28245=CARTESIAN_POINT('Ctrl Pts',(7.66048059708591,-15.7344445945251,0.0693026530250574));
#28246=CARTESIAN_POINT('Ctrl Pts',(7.73596042367391,-15.6972924318009,0.123164970119317));
#28247=CARTESIAN_POINT('Ctrl Pts',(7.74353659553707,-15.6935563226023,0.128845583461468));
#28248=CARTESIAN_POINT('Ctrl Pts',(7.75098709974897,-15.6898756840048,0.134720657333169));
#28249=CARTESIAN_POINT('',(7.75098748126849,-15.6898754955296,98.476464169983));
#28250=CARTESIAN_POINT('',(7.75098709974897,-15.6898756840048,0.));
#28251=CARTESIAN_POINT('',(7.62166407822415,-15.7531022199328,98.5000002325512));
#28252=CARTESIAN_POINT('Ctrl Pts',(7.75098827006064,-15.6898751058567,98.4764666117908));
#28253=CARTESIAN_POINT('Ctrl Pts',(7.7303651955325,-15.7000631543709,98.4847544570796));
#28254=CARTESIAN_POINT('Ctrl Pts',(7.70899812928377,-15.7105675084655,98.4906432907328));
#28255=CARTESIAN_POINT('Ctrl Pts',(7.66563449409477,-15.7317713310212,98.4982621653014));
#28256=CARTESIAN_POINT('Ctrl Pts',(7.64364124698376,-15.7424694536168,98.5000001531238));
#28257=CARTESIAN_POINT('Ctrl Pts',(7.62166492311255,-15.7531020373702,98.5000000867633));
#28258=CARTESIAN_POINT('',(3.09338542091476,-17.2244295086968,98.5000006225421));
#28259=CARTESIAN_POINT('Origin',(0.,0.,98.5));
#28260=CARTESIAN_POINT('Ctrl Pts',(3.09338528775829,-17.2244293798512,98.5000011593602));
#28261=CARTESIAN_POINT('Ctrl Pts',(3.06935680199565,-17.228744725382,98.5000018789964));
#28262=CARTESIAN_POINT('Ctrl Pts',(3.04527498726416,-17.2330171964727,98.4982647459742));
#28263=CARTESIAN_POINT('Ctrl Pts',(2.99772878170086,-17.241351622266,98.4906474053965));
#28264=CARTESIAN_POINT('Ctrl Pts',(2.97426775127848,-17.2454127370105,98.4847593539945));
#28265=CARTESIAN_POINT('Ctrl Pts',(2.95159454990794,-17.249292438038,98.4764721130871));
#28266=CARTESIAN_POINT('Origin',(0.,0.,0.));
#28267=CARTESIAN_POINT('',(-7.7509870154707,-15.6898756108788,98.4764611650906));
#28268=CARTESIAN_POINT('',(-7.75098709974897,-15.6898756840048,0.134720657333168));
#28269=CARTESIAN_POINT('',(-7.75098709974897,-15.6898756840048,0.));
#28270=CARTESIAN_POINT('',(-7.35749486474657,-15.8782010730192,5.26598123633362E-16));
#28271=CARTESIAN_POINT('Ctrl Pts',(-7.75098709974897,-15.6898756840048,
0.134720657333169));
#28272=CARTESIAN_POINT('Ctrl Pts',(-7.697365011278,-15.716365639972,0.0924371122250959));
#28273=CARTESIAN_POINT('Ctrl Pts',(-7.6352513765003,-15.7466976482487,0.0586496504523847));
#28274=CARTESIAN_POINT('Ctrl Pts',(-7.50029890429085,-15.8114252069992,
0.0120815387590078));
#28275=CARTESIAN_POINT('Ctrl Pts',(-7.42882654248637,-15.8451480558511,
1.30690686544886E-16));
#28276=CARTESIAN_POINT('Ctrl Pts',(-7.35749486474657,-15.8782010730192,
4.16333634234434E-16));
#28277=CARTESIAN_POINT('',(-3.38063404204883,-17.1703614834907,5.26598123633362E-16));
#28278=CARTESIAN_POINT('Origin',(0.,0.,5.26598123633362E-16));
#28279=CARTESIAN_POINT('',(-2.95159725048241,-17.2492919759318,0.134720657333156));
#28280=CARTESIAN_POINT('Ctrl Pts',(-3.38063404204883,-17.1703614834907,
4.22838847269347E-16));
#28281=CARTESIAN_POINT('Ctrl Pts',(-3.32758771379059,-17.180805656334,1.88689696034983E-16));
#28282=CARTESIAN_POINT('Ctrl Pts',(-3.27451359919498,-17.1909957556844,
0.00571187761951954));
#28283=CARTESIAN_POINT('Ctrl Pts',(-3.13564985748461,-17.2170134253201,
0.0353494158279846));
#28284=CARTESIAN_POINT('Ctrl Pts',(-3.05101549755282,-17.2321505944616,
0.0693026530250558));
#28285=CARTESIAN_POINT('Ctrl Pts',(-2.96811354177061,-17.2464597923539,
0.123164970119312));
#28286=CARTESIAN_POINT('Ctrl Pts',(-2.95978826009315,-17.2478903786094,
0.128845583461462));
#28287=CARTESIAN_POINT('Ctrl Pts',(-2.95159725048241,-17.2492919759318,
0.134720657333158));
#28288=CARTESIAN_POINT('',(-2.95159683426415,-17.2492920471526,98.4764641502857));
#28289=CARTESIAN_POINT('',(-2.95159725048241,-17.2492919759318,0.));
#28290=CARTESIAN_POINT('',(-3.09338455449681,-17.2244295302922,98.5000000582797));
#28291=CARTESIAN_POINT('Ctrl Pts',(-2.95159597373243,-17.2492921944017,
98.4764665733303));
#28292=CARTESIAN_POINT('Ctrl Pts',(-2.9742687703255,-17.245412560711,98.4847544660919));
#28293=CARTESIAN_POINT('Ctrl Pts',(-2.99772938956436,-17.2413515161255,
98.4906433246676));
#28294=CARTESIAN_POINT('Ctrl Pts',(-3.04527460155157,-17.2330172636463,
98.4982622140882));
#28295=CARTESIAN_POINT('Ctrl Pts',(-3.06935553227692,-17.2287449523538,
98.5000001907974));
#28296=CARTESIAN_POINT('Ctrl Pts',(-3.09338455123441,-17.2244295121256,
98.5000001151055));
#28297=CARTESIAN_POINT('',(-7.62166294207788,-15.7531030650529,98.5000002711098));
#28298=CARTESIAN_POINT('Origin',(0.,0.,98.5));
#28299=CARTESIAN_POINT('Ctrl Pts',(-7.62166291493897,-15.7531030089644,
98.5000005001312));
#28300=CARTESIAN_POINT('Ctrl Pts',(-7.64364355112194,-15.7424683422865,
98.5000007104308));
#28301=CARTESIAN_POINT('Ctrl Pts',(-7.66563431697665,-15.7317714169945,
98.4982623363923));
#28302=CARTESIAN_POINT('Ctrl Pts',(-7.70900073858256,-15.7105662332996,
98.4906410122901));
#28303=CARTESIAN_POINT('Ctrl Pts',(-7.73036164225108,-15.7000649076559,
98.4847522013256));
#28304=CARTESIAN_POINT('Ctrl Pts',(-7.75098699878812,-15.6898757338807,
98.4764609724326));
#28305=CARTESIAN_POINT('Origin',(0.,0.,0.));
#28306=CARTESIAN_POINT('',(-15.4929577055453,-8.137460149758,98.4764611351388));
#28307=CARTESIAN_POINT('',(-15.4929578242382,-8.13746016004849,0.134720657333155));
#28308=CARTESIAN_POINT('',(-15.4929578242382,-8.13746016004849,0.));
#28309=CARTESIAN_POINT('',(-15.2853108052616,-8.52110753285942,5.26598123633362E-16));
#28310=CARTESIAN_POINT('Ctrl Pts',(-15.4929578242382,-8.13746016004849,
0.134720657333155));
#28311=CARTESIAN_POINT('Ctrl Pts',(-15.4651470488427,-8.19040925740653,
0.0924371122251127));
#28312=CARTESIAN_POINT('Ctrl Pts',(-15.4327247698626,-8.25145784606452,
0.0586496504523958));
#28313=CARTESIAN_POINT('Ctrl Pts',(-15.3615918308627,-8.38314661402319,
0.0120815387590066));
#28314=CARTESIAN_POINT('Ctrl Pts',(-15.3235912687552,-8.45243937205836,
6.02511903288972E-17));
#28315=CARTESIAN_POINT('Ctrl Pts',(-15.2853108052616,-8.52110753285941,
4.16333634234434E-16));
#28316=CARTESIAN_POINT('',(-12.8274756483065,-11.9040274063908,5.26598123633362E-16));
#28317=CARTESIAN_POINT('Origin',(0.,0.,5.26598123633362E-16));
#28318=CARTESIAN_POINT('',(-12.5267717721302,-12.2200650149237,0.13472065733317));
#28319=CARTESIAN_POINT('Ctrl Pts',(-12.8274756483065,-11.9040274063908,
4.28259858131774E-16));
#28320=CARTESIAN_POINT('Ctrl Pts',(-12.7906991980261,-11.9436567691517,
-2.49978313375409E-16));
#28321=CARTESIAN_POINT('Ctrl Pts',(-12.7537509274744,-11.9830969145383,
0.00571187761951878));
#28322=CARTESIAN_POINT('Ctrl Pts',(-12.6567006030391,-12.0857677108831,
0.0353494158279818));
#28323=CARTESIAN_POINT('Ctrl Pts',(-12.597127372329,-12.1477607665704,0.0693026530250494));
#28324=CARTESIAN_POINT('Ctrl Pts',(-12.5384690167276,-12.2080656978362,
0.123164970119316));
#28325=CARTESIAN_POINT('Ctrl Pts',(-12.5325745998707,-12.21411654422,0.128845583461468));
#28326=CARTESIAN_POINT('Ctrl Pts',(-12.5267717721302,-12.2200650149237,
0.134720657333169));
#28327=CARTESIAN_POINT('',(-12.5267714753738,-12.2200653191283,98.4764641666045));
#28328=CARTESIAN_POINT('',(-12.5267717721302,-12.2200650149237,0.));
#28329=CARTESIAN_POINT('',(-12.6268663170877,-12.1166104030897,98.5000000583843));
#28330=CARTESIAN_POINT('Ctrl Pts',(-12.5267708618295,-12.2200659480716,
98.4764666051942));
#28331=CARTESIAN_POINT('Ctrl Pts',(-12.5428331499379,-12.2036005211659,
98.4847544881405));
#28332=CARTESIAN_POINT('Ctrl Pts',(-12.5594261690095,-12.1865252595175,
98.4906433390831));
#28333=CARTESIAN_POINT('Ctrl Pts',(-12.5929923076292,-12.1518363282392,
98.4982622190212));
#28334=CARTESIAN_POINT('Ctrl Pts',(-12.6099629957876,-12.1342255319367,
98.5000001912344));
#28335=CARTESIAN_POINT('Ctrl Pts',(-12.6268663036907,-12.1166103902338,
98.500000115428));
#28336=CARTESIAN_POINT('',(-15.4254964602665,-8.26462701674582,98.5000002246579));
#28337=CARTESIAN_POINT('Origin',(0.,0.,98.5));
#28338=CARTESIAN_POINT('Ctrl Pts',(-15.4254964408324,-8.26462700633653,
98.5000005203777));
#28339=CARTESIAN_POINT('Ctrl Pts',(-15.4370282602939,-8.2431034651139,98.5000007416218));
#28340=CARTESIAN_POINT('Ctrl Pts',(-15.448531655215,-8.2215236481436,98.4982623777968));
#28341=CARTESIAN_POINT('Ctrl Pts',(-15.4711517457392,-8.17887812715025,
98.4906410339747));
#28342=CARTESIAN_POINT('Ctrl Pts',(-15.4822605547265,-8.15782675347622,
98.4847521990827));
#28343=CARTESIAN_POINT('Ctrl Pts',(-15.4929577683353,-8.13746026648238,
98.47646092943));
#28344=CARTESIAN_POINT('Origin',(0.,0.,0.));
#28345=CARTESIAN_POINT('',(-17.3171451173558,2.52318944679938,98.4764669873977));
#28346=CARTESIAN_POINT('',(-17.3171452461371,2.52318856294819,0.134720657333157));
#28347=CARTESIAN_POINT('',(-17.3171452461371,2.52318856294819,0.));
#28348=CARTESIAN_POINT('',(-17.3746575467727,2.0907594630599,5.26598123633362E-16));
#28349=CARTESIAN_POINT('Ctrl Pts',(-17.3171452461371,2.52318856294819,0.134720657333156));
#28350=CARTESIAN_POINT('Ctrl Pts',(-17.3257685547646,2.46400507971636,0.0924371122250624));
#28351=CARTESIAN_POINT('Ctrl Pts',(-17.3354218401598,2.39555839657922,0.0586496504523668));
#28352=CARTESIAN_POINT('Ctrl Pts',(-17.3552787993477,2.24720905283605,0.0120815387590083));
#28353=CARTESIAN_POINT('Ctrl Pts',(-17.3652649600707,2.1688138640129,1.30690686544881E-16));
#28354=CARTESIAN_POINT('Ctrl Pts',(-17.3746575467727,2.0907594630599,4.16333634234434E-16));
#28355=CARTESIAN_POINT('',(-17.3746575467727,-2.0907594630599,5.26598123633362E-16));
#28356=CARTESIAN_POINT('Origin',(0.,0.,5.26598123633362E-16));
#28357=CARTESIAN_POINT('',(-17.3171452461371,-2.52318856294818,0.134720657333156));
#28358=CARTESIAN_POINT('Ctrl Pts',(-17.3746575467727,-2.0907594630599,4.36933475511658E-16));
#28359=CARTESIAN_POINT('Ctrl Pts',(-17.3681983284916,-2.14443694611619,
2.29452361695802E-16));
#28360=CARTESIAN_POINT('Ctrl Pts',(-17.3614888855091,-2.1980623425226,0.00571187761951909));
#28361=CARTESIAN_POINT('Ctrl Pts',(-17.3433219036639,-2.33816951102481,
0.0353494158279826));
#28362=CARTESIAN_POINT('Ctrl Pts',(-17.3315647514872,-2.42333921305186,
0.0693026530250511));
#28363=CARTESIAN_POINT('Ctrl Pts',(-17.3195554941821,-2.50660544363677,
0.123164970119312));
#28364=CARTESIAN_POINT('Ctrl Pts',(-17.3183434090412,-2.51496533249098,
0.128845583461461));
#28365=CARTESIAN_POINT('Ctrl Pts',(-17.3171452461371,-2.52318856294818,
0.134720657333157));
#28366=CARTESIAN_POINT('',(-17.3171451847825,-2.5231889840369,98.4764641699832));
#28367=CARTESIAN_POINT('',(-17.3171452461371,-2.52318856294818,0.));
#28368=CARTESIAN_POINT('',(-17.3373142437191,-2.38065698652274,98.5000002325512));
#28369=CARTESIAN_POINT('Ctrl Pts',(-17.3171450579317,-2.52318985463842,
98.4764666117912));
#28370=CARTESIAN_POINT('Ctrl Pts',(-17.3204615873541,-2.50042786509184,
98.48475445708));
#28371=CARTESIAN_POINT('Ctrl Pts',(-17.3238490351745,-2.47686055357152,
98.4906432907331));
#28372=CARTESIAN_POINT('Ctrl Pts',(-17.330614968575,-2.42906694423984,98.4982621653015));
#28373=CARTESIAN_POINT('Ctrl Pts',(-17.3339932006628,-2.40484422157081,
98.5000001531238));
#28374=CARTESIAN_POINT('Ctrl Pts',(-17.3373143311766,-2.38065784647426,
98.5000000867633));
#28375=CARTESIAN_POINT('',(-17.337314588927,2.38065707462717,98.5000006225421));
#28376=CARTESIAN_POINT('Origin',(0.,0.,98.5));
#28377=CARTESIAN_POINT('Ctrl Pts',(-17.3373144252399,2.38065716145103,98.5000011593602));
#28378=CARTESIAN_POINT('Ctrl Pts',(-17.3339933522773,2.4048431245179,98.5000018789964));
#28379=CARTESIAN_POINT('Ctrl Pts',(-17.3306150237413,2.42906655751751,98.4982647459742));
#28380=CARTESIAN_POINT('Ctrl Pts',(-17.3238489481646,2.47686116535221,98.4906474053964));
#28381=CARTESIAN_POINT('Ctrl Pts',(-17.3204614406997,2.50042888468654,98.4847593539945));
#28382=CARTESIAN_POINT('Ctrl Pts',(-17.3171448511027,2.5231912741458,98.476472113087));
#28383=CARTESIAN_POINT('Origin',(0.,17.5,2.63299061816681E-16));
#28384=CARTESIAN_POINT('Origin',(12.2482946431511,16.8583313034371,2.16840434497101E-16));
#28385=CARTESIAN_POINT('Origin',(19.8181570368417,6.43930956430664,2.16840434497101E-16));
#28386=CARTESIAN_POINT('Origin',(19.8181570368417,-6.43930956430665,2.16840434497101E-16));
#28387=CARTESIAN_POINT('Origin',(12.2482946431511,-16.8583313034371,2.16840434497101E-16));
#28388=CARTESIAN_POINT('Origin',(-2.55192432461455E-15,-20.8380434782609,
2.16840434497101E-16));
#28389=CARTESIAN_POINT('Origin',(-12.2482946431511,-16.8583313034371,2.16840434497101E-16));
#28390=CARTESIAN_POINT('Origin',(-19.8181570368417,-6.43930956430665,2.16840434497101E-16));
#28391=CARTESIAN_POINT('',(-15.2853108052616,8.52110753285942,5.26598123633362E-16));
#28392=CARTESIAN_POINT('Origin',(-19.8181570368417,6.43930956430665,2.16840434497101E-16));
#28393=CARTESIAN_POINT('',(-12.8274756483065,11.9040274063908,5.26598123633362E-16));
#28394=CARTESIAN_POINT('Origin',(0.,0.,5.26598123633362E-16));
#28395=CARTESIAN_POINT('Origin',(-12.2482946431511,16.8583313034371,2.16840434497101E-16));
#28396=CARTESIAN_POINT('Origin',(0.,20.8380434782609,2.16840434497101E-16));
#28397=CARTESIAN_POINT('',(15.,-1.83697019872103E-15,0.));
#28398=CARTESIAN_POINT('Origin',(0.,0.,0.));
#28399=CARTESIAN_POINT('Origin',(0.,0.,0.));
#28400=CARTESIAN_POINT('',(14.,0.,30.9));
#28401=CARTESIAN_POINT('Origin',(0.,0.,30.9));
#28402=CARTESIAN_POINT('',(14.,-1.71450551880629E-15,3.24999999999998));
#28403=CARTESIAN_POINT('',(14.,-1.71450551880629E-15,0.));
#28404=CARTESIAN_POINT('Origin',(0.,0.,3.24999999999998));
#28405=CARTESIAN_POINT('Origin',(0.,0.,0.));
#28406=CARTESIAN_POINT('',(14.,-1.71450551880629E-15,42.));
#28407=CARTESIAN_POINT('Origin',(0.,0.,42.));
#28408=CARTESIAN_POINT('',(14.,0.,32.8));
#28409=CARTESIAN_POINT('',(14.,-1.71450551880629E-15,0.));
#28410=CARTESIAN_POINT('Origin',(0.,0.,32.8));
#28411=CARTESIAN_POINT('Origin',(0.,0.,0.));
#28412=CARTESIAN_POINT('',(-12.5267717256653,12.22006490522,98.476461135139));
#28413=CARTESIAN_POINT('',(-12.5267717721302,12.2200650149237,0.134720657333155));
#28414=CARTESIAN_POINT('',(-12.5267717721302,12.2200650149237,0.));
#28415=CARTESIAN_POINT('Ctrl Pts',(-12.5267717721302,12.2200650149237,0.134720657333157));
#28416=CARTESIAN_POINT('Ctrl Pts',(-12.5685353539806,12.1772532248401,0.0924371122250874));
#28417=CARTESIAN_POINT('Ctrl Pts',(-12.6165769768332,12.127552753765,0.0586496504523806));
#28418=CARTESIAN_POINT('Ctrl Pts',(-12.7198391507123,12.0192072413384,0.0120815387590078));
#28419=CARTESIAN_POINT('Ctrl Pts',(-12.7739976602867,11.9616539193032,2.01130182760891E-16));
#28420=CARTESIAN_POINT('Ctrl Pts',(-12.8274756483065,11.9040274063908,4.16333634234434E-16));
#28421=CARTESIAN_POINT('',(-15.4929578242382,8.13746016004849,0.134720657333156));
#28422=CARTESIAN_POINT('Ctrl Pts',(-15.2853108052616,8.52110753285942,5.65953534037433E-16));
#28423=CARTESIAN_POINT('Ctrl Pts',(-15.3116360208225,8.47388490360466,3.69631386233599E-16));
#28424=CARTESIAN_POINT('Ctrl Pts',(-15.3377281845829,8.42655733494556,0.00571187761951948));
#28425=CARTESIAN_POINT('Ctrl Pts',(-15.4053837149197,8.30252997058624,0.0353494158279853));
#28426=CARTESIAN_POINT('Ctrl Pts',(-15.4459334737969,8.22671555358209,0.0693026530250567));
#28427=CARTESIAN_POINT('Ctrl Pts',(-15.485160442899,8.15229289364641,0.123164970119313));
#28428=CARTESIAN_POINT('Ctrl Pts',(-15.4890936648008,8.14481715572194,0.12884558346146));
#28429=CARTESIAN_POINT('Ctrl Pts',(-15.4929578242382,8.13746016004849,0.134720657333156));
#28430=CARTESIAN_POINT('',(-15.4929580205917,8.13745978620983,98.4764641502858));
#28431=CARTESIAN_POINT('',(-15.4929578242382,8.13746016004849,0.));
#28432=CARTESIAN_POINT('',(-15.4254975467744,8.26462498123528,98.5000000582797));
#28433=CARTESIAN_POINT('Ctrl Pts',(-15.4929584265529,8.13745901329798,98.4764665733304));
#28434=CARTESIAN_POINT('Ctrl Pts',(-15.4822623961932,8.15782325149825,98.4847544660921));
#28435=CARTESIAN_POINT('Ctrl Pts',(-15.4711503832337,8.17888069451006,98.4906433246677));
#28436=CARTESIAN_POINT('Ctrl Pts',(-15.4485317595999,8.22152345253713,98.4982622140882));
#28437=CARTESIAN_POINT('Ctrl Pts',(-15.4370271332712,8.24310556182703,98.5000001907974));
#28438=CARTESIAN_POINT('Ctrl Pts',(-15.4254975305051,8.26462497251878,98.5000001151055));
#28439=CARTESIAN_POINT('',(-12.626867931918,12.1166087252795,98.5000002246578));
#28440=CARTESIAN_POINT('Origin',(0.,0.,98.5));
#28441=CARTESIAN_POINT('Ctrl Pts',(-12.6268679160127,12.1166087100132,98.5000005203777));
#28442=CARTESIAN_POINT('Ctrl Pts',(-12.6099613400685,12.1342272620742,98.5000007416218));
#28443=CARTESIAN_POINT('Ctrl Pts',(-12.5929924590423,12.1518361709525,98.4982623777967));
#28444=CARTESIAN_POINT('Ctrl Pts',(-12.5594241507976,12.1865273461651,98.4906410339749));
#28445=CARTESIAN_POINT('Ctrl Pts',(-12.542835915452,12.2035976835611,98.484752199083));
#28446=CARTESIAN_POINT('Ctrl Pts',(-12.5267718560799,12.220064928867,98.4764609294303));
#28447=CARTESIAN_POINT('Origin',(0.,12.35,184.));
#28448=CARTESIAN_POINT('',(12.35,0.,184.));
#28449=CARTESIAN_POINT('Origin',(0.,0.,184.));
#28450=CARTESIAN_POINT('',(-11.35,-1.38997411703225E-15,184.));
#28451=CARTESIAN_POINT('Origin',(0.,0.,184.));
#28452=CARTESIAN_POINT('Origin',(0.,0.,161.));
#28453=CARTESIAN_POINT('',(13.,0.,161.));
#28454=CARTESIAN_POINT('',(-13.,-1.59204083889156E-15,161.));
#28455=CARTESIAN_POINT('Origin',(0.,0.,161.));
#28456=CARTESIAN_POINT('Origin',(0.,0.,161.));
#28457=CARTESIAN_POINT('',(13.,-1.59204083889156E-15,161.));
#28458=CARTESIAN_POINT('Origin',(0.,0.,0.));
#28459=CARTESIAN_POINT('',(-13.,-1.59204083889156E-15,111.));
#28460=CARTESIAN_POINT('',(-13.,-1.59204083889156E-15,0.));
#28461=CARTESIAN_POINT('Origin',(0.,0.,111.));
#28462=CARTESIAN_POINT('',(9.07821927770119,9.30515635258077,125.));
#28463=CARTESIAN_POINT('',(6.04440554879513,11.5093510486775,125.));
#28464=CARTESIAN_POINT('Ctrl Pts',(9.07821927770119,9.30515635258078,125.));
#28465=CARTESIAN_POINT('Ctrl Pts',(9.07821927770119,9.30515635258078,125.235784463582));
#28466=CARTESIAN_POINT('Ctrl Pts',(9.04424645795556,9.33867951762762,125.487056987681));
#28467=CARTESIAN_POINT('Ctrl Pts',(8.90448693202246,9.47203470845874,125.948918874434));
#28468=CARTESIAN_POINT('Ctrl Pts',(8.79848999736503,9.57154722295921,126.15953679602));
#28469=CARTESIAN_POINT('Ctrl Pts',(8.54947275134611,9.79461368903714,126.492111158983));
#28470=CARTESIAN_POINT('Ctrl Pts',(8.38972960894075,9.9330725460095,126.636358409655));
#28471=CARTESIAN_POINT('Ctrl Pts',(8.03108912785565,10.2252188501698,126.827811869943));
#28472=CARTESIAN_POINT('Ctrl Pts',(7.83195907934858,10.3786323587528,126.875));
#28473=CARTESIAN_POINT('Ctrl Pts',(7.45045748025558,10.6558094949959,126.875));
#28474=CARTESIAN_POINT('Ctrl Pts',(7.24301799415061,10.7977860438999,126.827811869943));
#28475=CARTESIAN_POINT('Ctrl Pts',(6.85434434434132,11.0485952376137,126.636358409655));
#28476=CARTESIAN_POINT('Ctrl Pts',(6.67329880044087,11.1577338543056,126.492111158983));
#28477=CARTESIAN_POINT('Ctrl Pts',(6.38419942339823,11.3256319999085,126.15953679602));
#28478=CARTESIAN_POINT('Ctrl Pts',(6.25680254386883,11.3956900171882,125.948918874434));
#28479=CARTESIAN_POINT('Ctrl Pts',(6.08678615200799,11.4874002047862,125.487056987681));
#28480=CARTESIAN_POINT('Ctrl Pts',(6.04440554879513,11.5093510486775,125.235784463582));
#28481=CARTESIAN_POINT('Ctrl Pts',(6.04440554879513,11.5093510486775,125.));
#28482=CARTESIAN_POINT('Ctrl Pts',(6.04440554879513,11.5093510486775,125.));
#28483=CARTESIAN_POINT('Ctrl Pts',(6.04440554879513,11.5093510486775,124.764215536418));
#28484=CARTESIAN_POINT('Ctrl Pts',(6.08678615200799,11.4874002047862,124.512943012319));
#28485=CARTESIAN_POINT('Ctrl Pts',(6.25680254386884,11.3956900171882,124.051081125566));
#28486=CARTESIAN_POINT('Ctrl Pts',(6.38419942339822,11.3256319999086,123.84046320398));
#28487=CARTESIAN_POINT('Ctrl Pts',(6.67329880044087,11.1577338543056,123.507888841017));
#28488=CARTESIAN_POINT('Ctrl Pts',(6.85434434434132,11.0485952376137,123.363641590345));
#28489=CARTESIAN_POINT('Ctrl Pts',(7.24301799415061,10.7977860438999,123.172188130057));
#28490=CARTESIAN_POINT('Ctrl Pts',(7.45045748025558,10.6558094949959,123.125));
#28491=CARTESIAN_POINT('Ctrl Pts',(7.83195907934858,10.3786323587528,123.125));
#28492=CARTESIAN_POINT('Ctrl Pts',(8.03108912785565,10.2252188501698,123.172188130057));
#28493=CARTESIAN_POINT('Ctrl Pts',(8.38972960894075,9.9330725460095,123.363641590345));
#28494=CARTESIAN_POINT('Ctrl Pts',(8.54947275134611,9.79461368903714,123.507888841017));
#28495=CARTESIAN_POINT('Ctrl Pts',(8.79848999736503,9.57154722295921,123.84046320398));
#28496=CARTESIAN_POINT('Ctrl Pts',(8.90448693202246,9.47203470845874,124.051081125566));
#28497=CARTESIAN_POINT('Ctrl Pts',(9.04424645795556,9.33867951762761,124.512943012319));
#28498=CARTESIAN_POINT('Ctrl Pts',(9.07821927770119,9.30515635258078,124.764215536418));
#28499=CARTESIAN_POINT('Ctrl Pts',(9.07821927770119,9.30515635258078,125.));
#28500=CARTESIAN_POINT('',(-6.04440554879529,11.5093510486774,125.));
#28501=CARTESIAN_POINT('',(-9.07821927770133,9.30515635258063,125.));
#28502=CARTESIAN_POINT('Ctrl Pts',(-6.0444055487953,11.5093510486774,125.));
#28503=CARTESIAN_POINT('Ctrl Pts',(-6.0444055487953,11.5093510486774,125.235784463582));
#28504=CARTESIAN_POINT('Ctrl Pts',(-6.08678615200817,11.4874002047861,125.487056987681));
#28505=CARTESIAN_POINT('Ctrl Pts',(-6.256802543869,11.3956900171881,125.948918874434));
#28506=CARTESIAN_POINT('Ctrl Pts',(-6.3841994233984,11.3256319999085,126.15953679602));
#28507=CARTESIAN_POINT('Ctrl Pts',(-6.67329880044104,11.1577338543055,126.492111158983));
#28508=CARTESIAN_POINT('Ctrl Pts',(-6.85434434434149,11.0485952376136,126.636358409655));
#28509=CARTESIAN_POINT('Ctrl Pts',(-7.24301799415078,10.7977860438998,126.827811869943));
#28510=CARTESIAN_POINT('Ctrl Pts',(-7.45045748025575,10.6558094949958,126.875));
#28511=CARTESIAN_POINT('Ctrl Pts',(-7.83195907934875,10.3786323587527,126.875));
#28512=CARTESIAN_POINT('Ctrl Pts',(-8.0310891278558,10.2252188501697,126.827811869943));
#28513=CARTESIAN_POINT('Ctrl Pts',(-8.3897296089409,9.93307254600937,126.636358409655));
#28514=CARTESIAN_POINT('Ctrl Pts',(-8.54947275134627,9.79461368903702,126.492111158983));
#28515=CARTESIAN_POINT('Ctrl Pts',(-8.79848999736518,9.57154722295908,126.15953679602));
#28516=CARTESIAN_POINT('Ctrl Pts',(-8.90448693202262,9.47203470845859,125.948918874434));
#28517=CARTESIAN_POINT('Ctrl Pts',(-9.04424645795571,9.33867951762747,125.487056987681));
#28518=CARTESIAN_POINT('Ctrl Pts',(-9.07821927770133,9.30515635258063,125.235784463582));
#28519=CARTESIAN_POINT('Ctrl Pts',(-9.07821927770133,9.30515635258063,125.));
#28520=CARTESIAN_POINT('Ctrl Pts',(-9.07821927770134,9.30515635258063,125.));
#28521=CARTESIAN_POINT('Ctrl Pts',(-9.07821927770134,9.30515635258063,124.764215536418));
#28522=CARTESIAN_POINT('Ctrl Pts',(-9.04424645795572,9.33867951762747,124.512943012319));
#28523=CARTESIAN_POINT('Ctrl Pts',(-8.90448693202261,9.4720347084586,124.051081125566));
#28524=CARTESIAN_POINT('Ctrl Pts',(-8.79848999736518,9.57154722295908,123.84046320398));
#28525=CARTESIAN_POINT('Ctrl Pts',(-8.54947275134627,9.79461368903702,123.507888841017));
#28526=CARTESIAN_POINT('Ctrl Pts',(-8.3897296089409,9.93307254600937,123.363641590345));
#28527=CARTESIAN_POINT('Ctrl Pts',(-8.0310891278558,10.2252188501697,123.172188130057));
#28528=CARTESIAN_POINT('Ctrl Pts',(-7.83195907934875,10.3786323587527,123.125));
#28529=CARTESIAN_POINT('Ctrl Pts',(-7.45045748025575,10.6558094949958,123.125));
#28530=CARTESIAN_POINT('Ctrl Pts',(-7.24301799415078,10.7977860438998,123.172188130057));
#28531=CARTESIAN_POINT('Ctrl Pts',(-6.85434434434149,11.0485952376136,123.363641590345));
#28532=CARTESIAN_POINT('Ctrl Pts',(-6.67329880044104,11.1577338543055,123.507888841017));
#28533=CARTESIAN_POINT('Ctrl Pts',(-6.3841994233984,11.3256319999085,123.84046320398));
#28534=CARTESIAN_POINT('Ctrl Pts',(-6.25680254386901,11.3956900171881,124.051081125566));
#28535=CARTESIAN_POINT('Ctrl Pts',(-6.08678615200816,11.4874002047862,124.512943012319));
#28536=CARTESIAN_POINT('Ctrl Pts',(-6.0444055487953,11.5093510486774,124.764215536418));
#28537=CARTESIAN_POINT('Ctrl Pts',(-6.0444055487953,11.5093510486774,125.));
#28538=CARTESIAN_POINT('',(-12.8138673486451,-2.19198621604393,125.));
#28539=CARTESIAN_POINT('',(-11.655053619739,-5.75844815215074,125.));
#28540=CARTESIAN_POINT('Ctrl Pts',(-12.8138673486451,-2.19198621604393,
125.));
#28541=CARTESIAN_POINT('Ctrl Pts',(-12.8138673486451,-2.19198621604393,
125.235784463582));
#28542=CARTESIAN_POINT('Ctrl Pts',(-12.8060871821488,-2.23907574869732,
125.487056987681));
#28543=CARTESIAN_POINT('Ctrl Pts',(-12.7714035650303,-2.42911095257868,
125.948918874434));
#28544=CARTESIAN_POINT('Ctrl Pts',(-12.7441422319827,-2.5719217029424,126.15953679602));
#28545=CARTESIAN_POINT('Ctrl Pts',(-12.6737982271025,-2.89875492965101,
126.492111158983));
#28546=CARTESIAN_POINT('Ctrl Pts',(-12.6259473843394,-3.1046651612241,126.636358409655));
#28547=CARTESIAN_POINT('Ctrl Pts',(-12.5075204293679,-3.55182007179051,
126.827811869943));
#28548=CARTESIAN_POINT('Ctrl Pts',(-12.4365950338825,-3.79297991320159,
126.875));
#28549=CARTESIAN_POINT('Ctrl Pts',(-12.2908743897914,-4.24146194054731,
126.875));
#28550=CARTESIAN_POINT('Ctrl Pts',(-12.2065040418452,-4.47825325208896,
126.827811869943));
#28551=CARTESIAN_POINT('Ctrl Pts',(-12.0394823990881,-4.90961879146154,
126.636358409655));
#28552=CARTESIAN_POINT('Ctrl Pts',(-11.9571635466639,-5.10432968780581,
126.492111158983));
#28553=CARTESIAN_POINT('Ctrl Pts',(-11.8219652914458,-5.41009049119521,
126.15953679602));
#28554=CARTESIAN_POINT('Ctrl Pts',(-11.760078120238,-5.54165062474212,125.948918874434));
#28555=CARTESIAN_POINT('Ctrl Pts',(-11.6764378656554,-5.71577885285004,
125.487056987681));
#28556=CARTESIAN_POINT('Ctrl Pts',(-11.655053619739,-5.75844815215074,125.235784463582));
#28557=CARTESIAN_POINT('Ctrl Pts',(-11.655053619739,-5.75844815215074,125.));
#28558=CARTESIAN_POINT('Ctrl Pts',(-11.655053619739,-5.75844815215074,125.));
#28559=CARTESIAN_POINT('Ctrl Pts',(-11.655053619739,-5.75844815215074,124.764215536418));
#28560=CARTESIAN_POINT('Ctrl Pts',(-11.6764378656554,-5.71577885285004,
124.512943012319));
#28561=CARTESIAN_POINT('Ctrl Pts',(-11.760078120238,-5.54165062474211,124.051081125566));
#28562=CARTESIAN_POINT('Ctrl Pts',(-11.8219652914458,-5.41009049119521,
123.84046320398));
#28563=CARTESIAN_POINT('Ctrl Pts',(-11.9571635466639,-5.10432968780581,
123.507888841017));
#28564=CARTESIAN_POINT('Ctrl Pts',(-12.0394823990881,-4.90961879146154,
123.363641590345));
#28565=CARTESIAN_POINT('Ctrl Pts',(-12.2065040418452,-4.47825325208896,
123.172188130057));
#28566=CARTESIAN_POINT('Ctrl Pts',(-12.2908743897914,-4.24146194054731,
123.125));
#28567=CARTESIAN_POINT('Ctrl Pts',(-12.4365950338825,-3.79297991320159,
123.125));
#28568=CARTESIAN_POINT('Ctrl Pts',(-12.5075204293679,-3.55182007179051,
123.172188130057));
#28569=CARTESIAN_POINT('Ctrl Pts',(-12.6259473843394,-3.10466516122411,
123.363641590345));
#28570=CARTESIAN_POINT('Ctrl Pts',(-12.6737982271025,-2.89875492965101,
123.507888841017));
#28571=CARTESIAN_POINT('Ctrl Pts',(-12.7441422319827,-2.57192170294239,
123.84046320398));
#28572=CARTESIAN_POINT('Ctrl Pts',(-12.7714035650303,-2.42911095257869,
124.051081125566));
#28573=CARTESIAN_POINT('Ctrl Pts',(-12.8060871821488,-2.23907574869732,
124.512943012319));
#28574=CARTESIAN_POINT('Ctrl Pts',(-12.8138673486451,-2.19198621604393,
124.764215536418));
#28575=CARTESIAN_POINT('Ctrl Pts',(-12.8138673486451,-2.19198621604393,
125.));
#28576=CARTESIAN_POINT('',(11.6550536197391,-5.75844815215058,125.));
#28577=CARTESIAN_POINT('',(12.8138673486451,-2.19198621604374,125.));
#28578=CARTESIAN_POINT('Ctrl Pts',(11.6550536197391,-5.75844815215058,125.));
#28579=CARTESIAN_POINT('Ctrl Pts',(11.6550536197391,-5.75844815215058,125.235784463582));
#28580=CARTESIAN_POINT('Ctrl Pts',(11.6764378656555,-5.71577885284987,125.487056987681));
#28581=CARTESIAN_POINT('Ctrl Pts',(11.7600781202381,-5.54165062474193,125.948918874434));
#28582=CARTESIAN_POINT('Ctrl Pts',(11.8219652914459,-5.41009049119505,126.15953679602));
#28583=CARTESIAN_POINT('Ctrl Pts',(11.957163546664,-5.10432968780564,126.492111158983));
#28584=CARTESIAN_POINT('Ctrl Pts',(12.0394823990882,-4.90961879146136,126.636358409655));
#28585=CARTESIAN_POINT('Ctrl Pts',(12.2065040418453,-4.47825325208878,126.827811869943));
#28586=CARTESIAN_POINT('Ctrl Pts',(12.2908743897914,-4.24146194054714,126.875));
#28587=CARTESIAN_POINT('Ctrl Pts',(12.4365950338825,-3.79297991320141,126.875));
#28588=CARTESIAN_POINT('Ctrl Pts',(12.5075204293679,-3.55182007179034,126.827811869943));
#28589=CARTESIAN_POINT('Ctrl Pts',(12.6259473843394,-3.10466516122393,126.636358409655));
#28590=CARTESIAN_POINT('Ctrl Pts',(12.6737982271026,-2.89875492965083,126.492111158983));
#28591=CARTESIAN_POINT('Ctrl Pts',(12.7441422319827,-2.57192170294221,126.15953679602));
#28592=CARTESIAN_POINT('Ctrl Pts',(12.7714035650303,-2.4291109525785,125.948918874434));
#28593=CARTESIAN_POINT('Ctrl Pts',(12.8060871821488,-2.23907574869713,125.487056987681));
#28594=CARTESIAN_POINT('Ctrl Pts',(12.8138673486451,-2.19198621604374,125.235784463582));
#28595=CARTESIAN_POINT('Ctrl Pts',(12.8138673486451,-2.19198621604374,125.));
#28596=CARTESIAN_POINT('Ctrl Pts',(12.8138673486451,-2.19198621604374,125.));
#28597=CARTESIAN_POINT('Ctrl Pts',(12.8138673486451,-2.19198621604374,124.764215536418));
#28598=CARTESIAN_POINT('Ctrl Pts',(12.8060871821488,-2.23907574869713,124.512943012319));
#28599=CARTESIAN_POINT('Ctrl Pts',(12.7714035650303,-2.42911095257849,124.051081125566));
#28600=CARTESIAN_POINT('Ctrl Pts',(12.7441422319827,-2.57192170294221,123.84046320398));
#28601=CARTESIAN_POINT('Ctrl Pts',(12.6737982271026,-2.89875492965083,123.507888841017));
#28602=CARTESIAN_POINT('Ctrl Pts',(12.6259473843394,-3.10466516122393,123.363641590345));
#28603=CARTESIAN_POINT('Ctrl Pts',(12.5075204293679,-3.55182007179033,123.172188130057));
#28604=CARTESIAN_POINT('Ctrl Pts',(12.4365950338825,-3.79297991320141,123.125));
#28605=CARTESIAN_POINT('Ctrl Pts',(12.2908743897914,-4.24146194054714,123.125));
#28606=CARTESIAN_POINT('Ctrl Pts',(12.2065040418453,-4.47825325208879,123.172188130057));
#28607=CARTESIAN_POINT('Ctrl Pts',(12.0394823990882,-4.90961879146136,123.363641590345));
#28608=CARTESIAN_POINT('Ctrl Pts',(11.957163546664,-5.10432968780564,123.507888841017));
#28609=CARTESIAN_POINT('Ctrl Pts',(11.8219652914459,-5.41009049119505,123.84046320398));
#28610=CARTESIAN_POINT('Ctrl Pts',(11.7600781202381,-5.54165062474194,124.051081125566));
#28611=CARTESIAN_POINT('Ctrl Pts',(11.6764378656555,-5.71577885284988,124.512943012319));
#28612=CARTESIAN_POINT('Ctrl Pts',(11.6550536197391,-5.75844815215058,124.764215536418));
#28613=CARTESIAN_POINT('Ctrl Pts',(11.6550536197391,-5.75844815215058,125.));
#28614=CARTESIAN_POINT('',(0.,-13.,126.875));
#28615=CARTESIAN_POINT('',(-2.29621274840127E-16,-13.,123.125));
#28616=CARTESIAN_POINT('Ctrl Pts',(1.38777878078145E-16,-13.,126.875));
#28617=CARTESIAN_POINT('Ctrl Pts',(0.23578095500191,-13.,126.875));
#28618=CARTESIAN_POINT('Ctrl Pts',(0.487054746182364,-12.9929315701904,
126.827811869943));
#28619=CARTESIAN_POINT('Ctrl Pts',(0.948920279348187,-12.9673838309378,
126.636358409655));
#28620=CARTESIAN_POINT('Ctrl Pts',(1.15953927046661,-12.9492629258861,126.492111158983));
#28621=CARTESIAN_POINT('Ctrl Pts',(1.49211363342996,-12.9151670287303,126.15953679602));
#28622=CARTESIAN_POINT('Ctrl Pts',(1.6363589433614,-12.8969631483263,125.948918874434));
#28623=CARTESIAN_POINT('Ctrl Pts',(1.82781098945425,-12.8712251208667,125.487056987681));
#28624=CARTESIAN_POINT('Ctrl Pts',(1.87499999999999,-12.8640730330638,125.235784463582));
#28625=CARTESIAN_POINT('Ctrl Pts',(1.87499999999999,-12.8640730330638,124.764215536418));
#28626=CARTESIAN_POINT('Ctrl Pts',(1.82781098945425,-12.8712251208667,124.512943012319));
#28627=CARTESIAN_POINT('Ctrl Pts',(1.63635894336139,-12.8969631483263,124.051081125566));
#28628=CARTESIAN_POINT('Ctrl Pts',(1.49211363342997,-12.9151670287303,123.84046320398));
#28629=CARTESIAN_POINT('Ctrl Pts',(1.15953927046661,-12.9492629258861,123.507888841017));
#28630=CARTESIAN_POINT('Ctrl Pts',(0.948920279348186,-12.9673838309378,
123.363641590345));
#28631=CARTESIAN_POINT('Ctrl Pts',(0.487054746182362,-12.9929315701904,
123.172188130057));
#28632=CARTESIAN_POINT('Ctrl Pts',(0.235780955001907,-13.,123.125));
#28633=CARTESIAN_POINT('Ctrl Pts',(-1.45716771982052E-15,-13.,123.125));
#28634=CARTESIAN_POINT('Ctrl Pts',(7.63278329429795E-16,-13.,123.125));
#28635=CARTESIAN_POINT('Ctrl Pts',(-0.235780955001908,-13.,123.125));
#28636=CARTESIAN_POINT('Ctrl Pts',(-0.487054746182362,-12.9929315701904,
123.172188130057));
#28637=CARTESIAN_POINT('Ctrl Pts',(-0.948920279348186,-12.9673838309378,
123.363641590345));
#28638=CARTESIAN_POINT('Ctrl Pts',(-1.15953927046661,-12.9492629258861,
123.507888841017));
#28639=CARTESIAN_POINT('Ctrl Pts',(-1.49211363342996,-12.9151670287303,
123.84046320398));
#28640=CARTESIAN_POINT('Ctrl Pts',(-1.63635894336139,-12.8969631483263,
124.051081125566));
#28641=CARTESIAN_POINT('Ctrl Pts',(-1.82781098945425,-12.8712251208667,
124.512943012319));
#28642=CARTESIAN_POINT('Ctrl Pts',(-1.87499999999999,-12.8640730330638,
124.764215536418));
#28643=CARTESIAN_POINT('Ctrl Pts',(-1.87499999999999,-12.8640730330638,
125.));
#28644=CARTESIAN_POINT('Ctrl Pts',(-1.87499999999999,-12.8640730330638,
125.235784463582));
#28645=CARTESIAN_POINT('Ctrl Pts',(-1.82781098945425,-12.8712251208667,
125.487056987681));
#28646=CARTESIAN_POINT('Ctrl Pts',(-1.6363589433614,-12.8969631483263,125.948918874434));
#28647=CARTESIAN_POINT('Ctrl Pts',(-1.49211363342996,-12.9151670287303,
126.15953679602));
#28648=CARTESIAN_POINT('Ctrl Pts',(-1.15953927046661,-12.9492629258861,
126.492111158983));
#28649=CARTESIAN_POINT('Ctrl Pts',(-0.948920279348187,-12.9673838309378,
126.636358409655));
#28650=CARTESIAN_POINT('Ctrl Pts',(-0.487054746182363,-12.9929315701904,
126.827811869943));
#28651=CARTESIAN_POINT('Ctrl Pts',(-0.235780955001909,-13.,126.875));
#28652=CARTESIAN_POINT('Ctrl Pts',(1.17961196366423E-15,-13.,126.875));
#28653=CARTESIAN_POINT('Origin',(0.,13.,111.));
#28654=CARTESIAN_POINT('',(-16.,-1.95943487863577E-15,111.));
#28655=CARTESIAN_POINT('Origin',(0.,0.,111.));
#28656=CARTESIAN_POINT('Origin',(0.,0.,0.));
#28657=CARTESIAN_POINT('',(-16.,-1.95943487863577E-15,100.));
#28658=CARTESIAN_POINT('',(-16.,-1.95943487863577E-15,0.));
#28659=CARTESIAN_POINT('',(16.,0.,100.));
#28660=CARTESIAN_POINT('Origin',(0.,0.,100.));
#28661=CARTESIAN_POINT('Origin',(0.,0.,100.));
#28662=CARTESIAN_POINT('Origin',(0.,0.,100.));
#28663=CARTESIAN_POINT('Ctrl Pts',(-7.62166314348063,15.7531022204317,98.500000610284));
#28664=CARTESIAN_POINT('Ctrl Pts',(-7.69400225181639,15.5188970106341,98.6793214334492));
#28665=CARTESIAN_POINT('Ctrl Pts',(-7.78580021647469,15.282866431888,98.8494491913713));
#28666=CARTESIAN_POINT('Ctrl Pts',(-8.01090275442514,14.8162420216974,99.1580199459299));
#28667=CARTESIAN_POINT('Ctrl Pts',(-8.14397944499903,14.5853179903069,99.2969308183713));
#28668=CARTESIAN_POINT('Ctrl Pts',(-8.38183223465004,14.242273311074,99.4748187550338));
#28669=CARTESIAN_POINT('Ctrl Pts',(-8.46796561908336,14.1280782793539,99.5290970577315));
#28670=CARTESIAN_POINT('Ctrl Pts',(-8.65039182617701,13.9063490976389,99.62326558462));
#28671=CARTESIAN_POINT('Ctrl Pts',(-8.74705976167071,13.7981959987251,99.6635148733605));
#28672=CARTESIAN_POINT('Ctrl Pts',(-9.05460506897777,13.4823163139724,99.7618768897715));
#28673=CARTESIAN_POINT('Ctrl Pts',(-9.28643675965965,13.2812823779052,99.7968963262704));
#28674=CARTESIAN_POINT('Ctrl Pts',(-9.6503936412052,13.0174883808938,99.7962149169054));
#28675=CARTESIAN_POINT('Ctrl Pts',(-9.775045002922,12.9350475934176,99.7875063317089));
#28676=CARTESIAN_POINT('Ctrl Pts',(-10.0309579794496,12.7810506313035,99.753358404991));
#28677=CARTESIAN_POINT('Ctrl Pts',(-10.1633841214783,12.708950911147,99.7275975989373));
#28678=CARTESIAN_POINT('Ctrl Pts',(-10.5613890038482,12.5136572830832,99.6277174576398));
#28679=CARTESIAN_POINT('Ctrl Pts',(-10.8257011162573,12.4115301467734,99.5324632749564));
#28680=CARTESIAN_POINT('Ctrl Pts',(-11.3534955337226,12.2529722492584,99.2974531785354));
#28681=CARTESIAN_POINT('Ctrl Pts',(-11.6189361780422,12.1966627203719,99.15615753822));
#28682=CARTESIAN_POINT('Ctrl Pts',(-12.1322393649622,12.1271244860313,98.8472990531188));
#28683=CARTESIAN_POINT('Ctrl Pts',(-12.3821304053377,12.1130390987287,98.6790582739387));
#28684=CARTESIAN_POINT('Ctrl Pts',(-12.6268678194693,12.1166087086112,98.5000000706302));
#28685=CARTESIAN_POINT('Ctrl Pts',(-15.4254975876205,8.26462497236944,98.5000000648311));
#28686=CARTESIAN_POINT('Ctrl Pts',(-15.3989615977616,8.18681012724391,98.5601400874486));
#28687=CARTESIAN_POINT('Ctrl Pts',(-15.3740814904822,8.1075208710261,98.6192489818091));
#28688=CARTESIAN_POINT('Ctrl Pts',(-15.350981847033,8.02689530039092,98.6770789349994));
#28689=CARTESIAN_POINT('Ctrl Pts',(-15.3272514958921,7.94406834653243,98.7364878647817));
#28690=CARTESIAN_POINT('Ctrl Pts',(-15.3053993169593,7.85983038415878,98.7945484303283));
#28691=CARTESIAN_POINT('Ctrl Pts',(-15.2855818246038,7.774281656423,98.8509939558039));
#28692=CARTESIAN_POINT('Ctrl Pts',(-15.2699513231154,7.70680745271355,98.8955138099879));
#28693=CARTESIAN_POINT('Ctrl Pts',(-15.2555868575626,7.63851671032234,98.9390292514823));
#28694=CARTESIAN_POINT('Ctrl Pts',(-15.2425795199652,7.56944243117125,98.981401669026));
#28695=CARTESIAN_POINT('Ctrl Pts',(-15.2403905735312,7.55781823091516,98.9885323328985));
#28696=CARTESIAN_POINT('Ctrl Pts',(-15.2382391277396,7.54617292290309,98.9956311576658));
#28697=CARTESIAN_POINT('Ctrl Pts',(-15.2361254605806,7.53450571055505,99.0026979840552));
#28698=CARTESIAN_POINT('Ctrl Pts',(-15.209459094505,7.38731027619741,99.0918542065433));
#28699=CARTESIAN_POINT('Ctrl Pts',(-15.1888463312715,7.2368487771976,99.1757821758939));
#28700=CARTESIAN_POINT('Ctrl Pts',(-15.1749739382223,7.08263617809772,99.2535679557348));
#28701=CARTESIAN_POINT('Ctrl Pts',(-15.1657087941053,6.97964010883575,99.3055198041236));
#28702=CARTESIAN_POINT('Ctrl Pts',(-15.1594497290289,6.87497109524008,99.3547324640411));
#28703=CARTESIAN_POINT('Ctrl Pts',(-15.1563931490129,6.7684890497211,99.4009428779259));
#28704=CARTESIAN_POINT('Ctrl Pts',(-15.1561145921655,6.75878496779186,99.405154194868));
#28705=CARTESIAN_POINT('Ctrl Pts',(-15.1558636606571,6.74906375936666,99.409340145667));
#28706=CARTESIAN_POINT('Ctrl Pts',(-15.1556404821766,6.73932606051682,99.4135002521259));
#28707=CARTESIAN_POINT('Ctrl Pts',(-15.1519973739088,6.58037036234059,99.4814087628382));
#28708=CARTESIAN_POINT('Ctrl Pts',(-15.1557666604111,6.41694578086669,99.5424448370954));
#28709=CARTESIAN_POINT('Ctrl Pts',(-15.1675209018535,6.25170583473857,99.5945560958749));
#28710=CARTESIAN_POINT('Ctrl Pts',(-15.1758230391991,6.13499522142745,99.6313627949514));
#28711=CARTESIAN_POINT('Ctrl Pts',(-15.1881085912407,6.01737791060435,99.6637177718552));
#28712=CARTESIAN_POINT('Ctrl Pts',(-15.2045787950897,5.89977535028896,99.6909054353086));
#28713=CARTESIAN_POINT('Ctrl Pts',(-15.2053629424751,5.89417628539394,99.6921998415835));
#28714=CARTESIAN_POINT('Ctrl Pts',(-15.2061565022706,5.88857599398075,99.6934831334187));
#28715=CARTESIAN_POINT('Ctrl Pts',(-15.2069595049574,5.8829744697482,99.694755268259));
#28716=CARTESIAN_POINT('Ctrl Pts',(-15.2273306528143,5.74087098709944,99.7270276969224));
#28717=CARTESIAN_POINT('Ctrl Pts',(-15.253773829766,5.59800970804938,99.7521123711275));
#28718=CARTESIAN_POINT('Ctrl Pts',(-15.2867992989703,5.45419637581596,99.7693348591779));
#28719=CARTESIAN_POINT('Ctrl Pts',(-15.2874528993659,5.45135019518315,99.7696757059629));
#28720=CARTESIAN_POINT('Ctrl Pts',(-15.2881090485027,5.44850399099787,99.7700133667743));
#28721=CARTESIAN_POINT('Ctrl Pts',(-15.2887677380553,5.44565779119462,99.7703478403197));
#28722=CARTESIAN_POINT('Ctrl Pts',(-15.3138490822817,5.33728121725203,99.7830838038606));
#28723=CARTESIAN_POINT('Ctrl Pts',(-15.3426027353379,5.22896570099945,99.7911914401022));
#28724=CARTESIAN_POINT('Ctrl Pts',(-15.3745952689208,5.1221752573672,99.794599167721));
#28725=CARTESIAN_POINT('Ctrl Pts',(-15.3858966024805,5.08445162971674,99.795802944421));
#28726=CARTESIAN_POINT('Ctrl Pts',(-15.3976023968509,5.04691831198085,99.7964198693814));
#28727=CARTESIAN_POINT('Ctrl Pts',(-15.4096944350009,5.00964014842566,99.7964455441609));
#28728=CARTESIAN_POINT('Ctrl Pts',(-15.4097526805227,5.00946058514124,99.7964456678324));
#28729=CARTESIAN_POINT('Ctrl Pts',(-15.4098109349276,5.00928102801947,99.7964457777851));
#28730=CARTESIAN_POINT('Ctrl Pts',(-15.4098691982134,5.00910147706792,99.7964458740184));
#28731=CARTESIAN_POINT('Ctrl Pts',(-15.452400154641,4.87803311074117,99.7965161223064));
#28732=CARTESIAN_POINT('Ctrl Pts',(-15.5000808965492,4.74882134911773,99.7893191842779));
#28733=CARTESIAN_POINT('Ctrl Pts',(-15.5525709850149,4.6220096743371,99.7751251055994));
#28734=CARTESIAN_POINT('Ctrl Pts',(-15.6056842522426,4.493692451656,99.7607625103754));
#28735=CARTESIAN_POINT('Ctrl Pts',(-15.6637220710125,4.3678319517557,99.7392354386705));
#28736=CARTESIAN_POINT('Ctrl Pts',(-15.7263585380238,4.24501089848265,99.7107825845669));
#28737=CARTESIAN_POINT('Ctrl Pts',(-15.7366180361955,4.22489350630477,99.7061221683815));
#28738=CARTESIAN_POINT('Ctrl Pts',(-15.7470009608383,4.20485771388323,99.701275858843));
#28739=CARTESIAN_POINT('Ctrl Pts',(-15.7575059376538,4.18490615157863,99.6962446073889));
#28740=CARTESIAN_POINT('Ctrl Pts',(-15.7603333207195,4.1795362483047,99.6948904611199));
#28741=CARTESIAN_POINT('Ctrl Pts',(-15.7631694550508,4.17417259583829,99.6935229664922));
#28742=CARTESIAN_POINT('Ctrl Pts',(-15.7660143095016,4.16881525076369,99.692142145394));
#28743=CARTESIAN_POINT('Ctrl Pts',(-15.8523453645961,4.00623918200715,99.6502392134979));
#28744=CARTESIAN_POINT('Ctrl Pts',(-15.945957559091,3.85094812019755,99.5964381242811));
#28745=CARTESIAN_POINT('Ctrl Pts',(-16.0446983463237,3.70416010938547,99.5332547186234));
#28746=CARTESIAN_POINT('Ctrl Pts',(-16.1016422036435,3.6195073961736,99.4968168195791));
#28747=CARTESIAN_POINT('Ctrl Pts',(-16.1602914482781,3.53768342281066,99.4572586816833));
#28748=CARTESIAN_POINT('Ctrl Pts',(-16.2202297140019,3.45892855318697,99.4150655759484));
#28749=CARTESIAN_POINT('Ctrl Pts',(-16.2263505132198,3.4508862326663,99.4107568839056));
#28750=CARTESIAN_POINT('Ctrl Pts',(-16.2324843106259,3.44287636886361,99.4064210546897));
#28751=CARTESIAN_POINT('Ctrl Pts',(-16.238630726799,3.43489911689116,99.4020585662807));
#28752=CARTESIAN_POINT('Ctrl Pts',(-16.3058910028174,3.34760399166231,99.3543198245074));
#28753=CARTESIAN_POINT('Ctrl Pts',(-16.3750790005671,3.2636136741201,99.3031450764238));
#28754=CARTESIAN_POINT('Ctrl Pts',(-16.4459839896838,3.1827936689064,99.2489133667349));
#28755=CARTESIAN_POINT('Ctrl Pts',(-16.5207937966315,3.09752281472716,99.1916950555439));
#28756=CARTESIAN_POINT('Ctrl Pts',(-16.5975155631586,3.01578072195888,99.1310729372186));
#28757=CARTESIAN_POINT('Ctrl Pts',(-16.6759149977342,2.9374575563625,99.0674634405586));
#28758=CARTESIAN_POINT('Ctrl Pts',(-16.7020156296198,2.91138231584061,99.0462866544537));
#28759=CARTESIAN_POINT('Ctrl Pts',(-16.7283022642725,2.88568641273419,99.0247785979167));
#28760=CARTESIAN_POINT('Ctrl Pts',(-16.7547663508278,2.86036698978197,99.0029542627797));
#28761=CARTESIAN_POINT('Ctrl Pts',(-16.8153481932165,2.80240552236248,98.9529937841234));
#28762=CARTESIAN_POINT('Ctrl Pts',(-16.8765673950408,2.74668841444285,98.9016192560261));
#28763=CARTESIAN_POINT('Ctrl Pts',(-16.9384055914951,2.69304838623785,98.8489571073848));
#28764=CARTESIAN_POINT('Ctrl Pts',(-17.0035287415344,2.63655890554152,98.7934974529318));
#28765=CARTESIAN_POINT('Ctrl Pts',(-17.06933900837,2.58237266537676,98.7366089356619));
#28766=CARTESIAN_POINT('Ctrl Pts',(-17.1358266349123,2.53034639929748,98.6784119085642));
#28767=CARTESIAN_POINT('Ctrl Pts',(-17.2023142614546,2.4783201332182,98.6202148814666));
#28768=CARTESIAN_POINT('Ctrl Pts',(-17.2694800239621,2.42845385999384,98.5607082197099));
#28769=CARTESIAN_POINT('Ctrl Pts',(-17.337314796066,2.38065715175377,98.5000007932762));
#28770=CARTESIAN_POINT('Ctrl Pts',(-17.3373139553419,-2.38065609737471,
98.500000610284));
#28771=CARTESIAN_POINT('Ctrl Pts',(-17.1369255782473,-2.52182806773903,
98.6793214334492));
#28772=CARTESIAN_POINT('Ctrl Pts',(-16.9408142894144,-2.68207058023464,
98.8494491913713));
#28773=CARTESIAN_POINT('Ctrl Pts',(-16.5665886131438,-3.0403506885261,99.1580199459299));
#28774=CARTESIAN_POINT('Ctrl Pts',(-16.3880897672633,-3.23827359237263,
99.2969308183713));
#28775=CARTESIAN_POINT('Ctrl Pts',(-16.1353354438601,-3.57049167360208,
99.4748187550338));
#28776=CARTESIAN_POINT('Ctrl Pts',(-16.0533461943871,-3.68769759561264,
99.5290970577315));
#28777=CARTESIAN_POINT('Ctrl Pts',(-15.8988420094755,-3.92971331391084,
99.62326558462));
#28778=CARTESIAN_POINT('Ctrl Pts',(-15.8258543348747,-4.05507112943762,
99.6635148733605));
#28779=CARTESIAN_POINT('Ctrl Pts',(-15.6204716288236,-4.44517628877436,
99.7618768897716));
#28780=CARTESIAN_POINT('Ctrl Pts',(-15.5009169261858,-4.72778423157193,
99.7968963262704));
#28781=CARTESIAN_POINT('Ctrl Pts',(-15.3625027879858,-5.15544462350693,
99.7962149169053));
#28782=CARTESIAN_POINT('Ctrl Pts',(-15.3226163289905,-5.29947071769255,
99.7875063317089));
#28783=CARTESIAN_POINT('Ctrl Pts',(-15.2552379735104,-5.59044609999894,
99.753358404991));
#28784=CARTESIAN_POINT('Ctrl Pts',(-15.2275889932189,-5.73867088412122,
99.7275975989373));
#28785=CARTESIAN_POINT('Ctrl Pts',(-15.1648439881543,-6.17754507098127,
99.6277174576398));
#28786=CARTESIAN_POINT('Ctrl Pts',(-15.14939224423,-6.46047984853023,99.5324632749564));
#28787=CARTESIAN_POINT('Ctrl Pts',(-15.1616921671213,-7.01143925344933,
99.2974531785354));
#28788=CARTESIAN_POINT('Ctrl Pts',(-15.1901642928368,-7.28128890929021,
99.15615753822));
#28789=CARTESIAN_POINT('Ctrl Pts',(-15.2826489099606,-7.79095774621569,
98.8472990531188));
#28790=CARTESIAN_POINT('Ctrl Pts',(-15.3464734888,-8.03297087257737,98.6790582739387));
#28791=CARTESIAN_POINT('Ctrl Pts',(-15.4254964096654,-8.26462691495154,
98.5000000706302));
#28792=CARTESIAN_POINT('Ctrl Pts',(-12.6268663212258,-12.1166104449802,
98.5000000648703));
#28793=CARTESIAN_POINT('Ctrl Pts',(-12.5446458774943,-12.1154191815706,
98.5601503317705));
#28794=CARTESIAN_POINT('Ctrl Pts',(-12.4615341179103,-12.1162591862576,
98.6192693642505));
#28795=CARTESIAN_POINT('Ctrl Pts',(-12.3777014366231,-12.1192061781956,
98.6771089720691));
#28796=CARTESIAN_POINT('Ctrl Pts',(-12.291574122314,-12.1222338339619,98.736531741395));
#28797=CARTESIAN_POINT('Ctrl Pts',(-12.2046849293976,-12.1274848184644,
98.7946054582262));
#28798=CARTESIAN_POINT('Ctrl Pts',(-12.117178171504,-12.1350769190544,98.8510630180339));
#28799=CARTESIAN_POINT('Ctrl Pts',(-12.0477278724933,-12.1411024383261,
98.8958709220683));
#28800=CARTESIAN_POINT('Ctrl Pts',(-11.9778875804926,-12.1486032210726,
98.9396611167543));
#28801=CARTESIAN_POINT('Ctrl Pts',(-11.9077182330857,-12.157657152302,98.9822921355006));
#28802=CARTESIAN_POINT('Ctrl Pts',(-11.8959551442278,-12.1591749403604,
98.9894387383999));
#28803=CARTESIAN_POINT('Ctrl Pts',(-11.8841835086262,-12.1607351471297,
98.9965533320491));
#28804=CARTESIAN_POINT('Ctrl Pts',(-11.872402649482,-12.1623382885869,99.0036357543382));
#28805=CARTESIAN_POINT('Ctrl Pts',(-11.7229964864066,-12.1826695064605,
99.0934558197971));
#28806=CARTESIAN_POINT('Ctrl Pts',(-11.5723364223253,-12.2098752720322,
99.1779621201775));
#28807=CARTESIAN_POINT('Ctrl Pts',(-11.4201636558614,-12.2447803502433,
99.256219095195));
#28808=CARTESIAN_POINT('Ctrl Pts',(-11.3200139898558,-12.2677524759789,
99.3077224626682));
#28809=CARTESIAN_POINT('Ctrl Pts',(-11.2192092246076,-12.2940588050411,
99.3565196706126));
#28810=CARTESIAN_POINT('Ctrl Pts',(-11.1176771661422,-12.3239257557744,
99.4023528281028));
#28811=CARTESIAN_POINT('Ctrl Pts',(-11.1083271026094,-12.3266761962865,
99.4065735928634));
#28812=CARTESIAN_POINT('Ctrl Pts',(-11.0989693146526,-12.3294584306974,
99.4107687371792));
#28813=CARTESIAN_POINT('Ctrl Pts',(-11.0896044489173,-12.332272384062,99.4149377803026));
#28814=CARTESIAN_POINT('Ctrl Pts',(-10.9368635549275,-12.3781679435612,
99.4829348441968));
#28815=CARTESIAN_POINT('Ctrl Pts',(-10.7821807783801,-12.4325386244579,
99.5439998059001));
#28816=CARTESIAN_POINT('Ctrl Pts',(-10.6282589265402,-12.4951094361099,
99.596075947797));
#28817=CARTESIAN_POINT('Ctrl Pts',(-10.5197442278578,-12.5392217742319,
99.6327895578461));
#28818=CARTESIAN_POINT('Ctrl Pts',(-10.4116066693124,-12.587410060724,99.6650361416381));
#28819=CARTESIAN_POINT('Ctrl Pts',(-10.3047803019272,-12.6395820517603,
99.6921021736602));
#28820=CARTESIAN_POINT('Ctrl Pts',(-10.2996691247951,-12.6420782546552,
99.6933971655926));
#28821=CARTESIAN_POINT('Ctrl Pts',(-10.2945597086435,-12.644583905749,99.6946809027462));
#28822=CARTESIAN_POINT('Ctrl Pts',(-10.2894520568858,-12.6470990367868,
99.6959533416379));
#28823=CARTESIAN_POINT('Ctrl Pts',(-10.1603732160565,-12.7106605743163,
99.7281099852292));
#28824=CARTESIAN_POINT('Ctrl Pts',(-10.0324732032076,-12.7802460636459,
99.753042557793));
#28825=CARTESIAN_POINT('Ctrl Pts',(-9.9057096702643,-12.8564220781232,99.7700686162087));
#28826=CARTESIAN_POINT('Ctrl Pts',(-9.78852854268104,-12.9268397373978,
99.7858076278718));
#28827=CARTESIAN_POINT('Ctrl Pts',(-9.67313030469678,-13.0025204956137,
99.7945520991956));
#28828=CARTESIAN_POINT('Ctrl Pts',(-9.56184140648273,-13.0818662612157,
99.7961709162458));
#28829=CARTESIAN_POINT('Ctrl Pts',(-9.5479606610537,-13.0917628312318,99.7963728266585));
#28830=CARTESIAN_POINT('Ctrl Pts',(-9.53414386521357,-13.1017164514468,
99.7964638312961));
#28831=CARTESIAN_POINT('Ctrl Pts',(-9.52039555682255,-13.1117240463959,
99.7964436301271));
#28832=CARTESIAN_POINT('Ctrl Pts',(-9.520267099632,-13.1118175522654,99.7964434413776));
#28833=CARTESIAN_POINT('Ctrl Pts',(-9.52013864842916,-13.11191106284,99.7964432429204));
#28834=CARTESIAN_POINT('Ctrl Pts',(-9.52001020321784,-13.1120045781169,
99.7964430347553));
#28835=CARTESIAN_POINT('Ctrl Pts',(-9.39854187906109,-13.2004402920585,
99.7962461766987));
#28836=CARTESIAN_POINT('Ctrl Pts',(-9.28143127084363,-13.2936651206149,
99.7875210116457));
#28837=CARTESIAN_POINT('Ctrl Pts',(-9.16861451193018,-13.3916016257417,
99.7704440514026));
#28838=CARTESIAN_POINT('Ctrl Pts',(-9.16621596908933,-13.3936838066649,
99.7700809863657));
#28839=CARTESIAN_POINT('Ctrl Pts',(-9.16381939232461,-13.39576809596,99.7697141495904));
#28840=CARTESIAN_POINT('Ctrl Pts',(-9.16142477903311,-13.3978544944897,
99.7693435426227));
#28841=CARTESIAN_POINT('Ctrl Pts',(-9.07547278649159,-13.4727434594413,
99.7560410158919));
#28842=CARTESIAN_POINT('Ctrl Pts',(-8.9915392882287,-13.5509036748962,99.7376874829348));
#28843=CARTESIAN_POINT('Ctrl Pts',(-8.91103700467454,-13.6308471455214,
99.7148306067551));
#28844=CARTESIAN_POINT('Ctrl Pts',(-8.88817991952993,-13.6535455664129,
99.7083408335225));
#28845=CARTESIAN_POINT('Ctrl Pts',(-8.86559966104437,-13.6763878102703,
99.7014877883099));
#28846=CARTESIAN_POINT('Ctrl Pts',(-8.84332918088635,-13.6993398531878,
99.6942835087754));
#28847=CARTESIAN_POINT('Ctrl Pts',(-8.83915122841372,-13.7036456671523,
99.692931982572));
#28848=CARTESIAN_POINT('Ctrl Pts',(-8.83498423109444,-13.707955266888,99.6915681321741));
#28849=CARTESIAN_POINT('Ctrl Pts',(-8.83082841847428,-13.712268414179,99.6901920420673));
#28850=CARTESIAN_POINT('Ctrl Pts',(-8.69127076580918,-13.8571095719862,
99.6439811267264));
#28851=CARTESIAN_POINT('Ctrl Pts',(-8.56417600543209,-14.0055185188973,
99.5845379976685));
#28852=CARTESIAN_POINT('Ctrl Pts',(-8.44794279560312,-14.1572127309531,
99.5138249402946));
#28853=CARTESIAN_POINT('Ctrl Pts',(-8.39715446235132,-14.2234958199739,
99.4829267286007));
#28854=CARTESIAN_POINT('Ctrl Pts',(-8.34843948408571,-14.2904060698911,
99.4498772977175));
#28855=CARTESIAN_POINT('Ctrl Pts',(-8.30166232922775,-14.357919515952,99.4148427913138));
#28856=CARTESIAN_POINT('Ctrl Pts',(-8.29602633367793,-14.3660539457331,
99.4106216213264));
#28857=CARTESIAN_POINT('Ctrl Pts',(-8.29041845450117,-14.3741972107076,
99.4063715743575));
#28858=CARTESIAN_POINT('Ctrl Pts',(-8.28483845220995,-14.3823492736635,
99.4020929385903));
#28859=CARTESIAN_POINT('Ctrl Pts',(-8.19855951863415,-14.5083978416683,
99.3359359530035));
#28860=CARTESIAN_POINT('Ctrl Pts',(-8.11890479704849,-14.6370031608812,
99.2625264797838));
#28861=CARTESIAN_POINT('Ctrl Pts',(-8.04618036364231,-14.7663488924165,
99.1837466668059));
#28862=CARTESIAN_POINT('Ctrl Pts',(-7.99257245587884,-14.8616944829006,
99.1256751116222));
#28863=CARTESIAN_POINT('Ctrl Pts',(-7.94273055714886,-14.9574417704728,
99.0646859940682));
#28864=CARTESIAN_POINT('Ctrl Pts',(-7.89678243508448,-15.052850115494,99.0015448475648));
#28865=CARTESIAN_POINT('Ctrl Pts',(-7.8916489520208,-15.0635094656762,98.9944905003656));
#28866=CARTESIAN_POINT('Ctrl Pts',(-7.88656339889997,-15.074165771925,98.9874085551186));
#28867=CARTESIAN_POINT('Ctrl Pts',(-7.88152602873833,-15.0848179083459,
98.9803001233707));
#28868=CARTESIAN_POINT('Ctrl Pts',(-7.82583177604172,-15.2025902297257,
98.9017077663791));
#28869=CARTESIAN_POINT('Ctrl Pts',(-7.77556907089792,-15.3204628413257,
98.8195805048243));
#28870=CARTESIAN_POINT('Ctrl Pts',(-7.7303783531495,-15.4384372752834,98.7343244488909));
#28871=CARTESIAN_POINT('Ctrl Pts',(-7.69023139128725,-15.5432445307731,
98.6585838588623));
#28872=CARTESIAN_POINT('Ctrl Pts',(-7.65408652108198,-15.6481322437112,
98.5803745642925));
#28873=CARTESIAN_POINT('Ctrl Pts',(-7.62166303813141,-15.7531031392177,
98.5000003292224));
#28874=CARTESIAN_POINT('Ctrl Pts',(-3.09338453344274,-17.2244295663994,
98.5000000648311));
#28875=CARTESIAN_POINT('Ctrl Pts',(-3.02757828977043,-17.175146230785,98.5601400874298));
#28876=CARTESIAN_POINT('Ctrl Pts',(-2.95985810196491,-17.1269821150027,
98.6192489817723));
#28877=CARTESIAN_POINT('Ctrl Pts',(-2.89031681004483,-17.0800983770824,
98.6770789349455));
#28878=CARTESIAN_POINT('Ctrl Pts',(-2.8188767776614,-17.0319345356753,98.7364878647103));
#28879=CARTESIAN_POINT('Ctrl Pts',(-2.74551440930578,-16.9851209165741,
98.7945484302403));
#28880=CARTESIAN_POINT('Ctrl Pts',(-2.67027667628172,-16.9398373506274,
98.8509939557004));
#28881=CARTESIAN_POINT('Ctrl Pts',(-2.61093498570845,-16.9041211846764,
98.8955138099206));
#28882=CARTESIAN_POINT('Ctrl Pts',(-2.55042549407967,-16.8693567661241,
98.9390292514498));
#28883=CARTESIAN_POINT('Ctrl Pts',(-2.48875143910593,-16.8356409267845,
98.9814016690262));
#28884=CARTESIAN_POINT('Ctrl Pts',(-2.47837258935355,-16.8299670395895,
98.9885323328987));
#28885=CARTESIAN_POINT('Ctrl Pts',(-2.46796207659648,-16.8243222949694,
98.995631157666));
#28886=CARTESIAN_POINT('Ctrl Pts',(-2.45751905733843,-16.8187067111521,
99.0026979840554));
#28887=CARTESIAN_POINT('Ctrl Pts',(-2.32576824024065,-16.7478595990157,
99.0918542067995));
#28888=CARTESIAN_POINT('Ctrl Pts',(-2.18904054489823,-16.6817605358573,
99.1757821763761));
#28889=CARTESIAN_POINT('Ctrl Pts',(-2.04666245239284,-16.620912792038,99.2535679564052));
#28890=CARTESIAN_POINT('Ctrl Pts',(-1.95157045694327,-16.5802735807903,
99.305519804547));
#28891=CARTESIAN_POINT('Ctrl Pts',(-1.85395846739465,-16.5419763523534,
99.3547324642399));
#28892=CARTESIAN_POINT('Ctrl Pts',(-1.75363255973665,-16.5061646105045,
99.400942877926));
#28893=CARTESIAN_POINT('Ctrl Pts',(-1.74448950818291,-16.5029009609687,
99.405154194868));
#28894=CARTESIAN_POINT('Ctrl Pts',(-1.7353216316644,-16.4996582923132,99.409340145667));
#28895=CARTESIAN_POINT('Ctrl Pts',(-1.72612949566279,-16.4964369225343,
99.4135002521259));
#28896=CARTESIAN_POINT('Ctrl Pts',(-1.57607942543336,-16.4438521085721,
99.4814087628581));
#28897=CARTESIAN_POINT('Ctrl Pts',(-1.4194886386662,-16.396935940076,99.5424448371308));
#28898=CARTESIAN_POINT('Ctrl Pts',(-1.25870385073772,-16.3570529364832,
99.5945560959203));
#28899=CARTESIAN_POINT('Ctrl Pts',(-1.14513995994311,-16.3288831753824,
99.6313627949779));
#28900=CARTESIAN_POINT('Ctrl Pts',(-1.0294828057368,-16.3042216818427,99.6637177718662));
#28901=CARTESIAN_POINT('Ctrl Pts',(-0.912546551574103,-16.283544586827,
99.6909054353085));
#28902=CARTESIAN_POINT('Ctrl Pts',(-0.906979209552365,-16.2825601491024,
99.6921998415834));
#28903=CARTESIAN_POINT('Ctrl Pts',(-0.901407792447838,-16.2815842840969,
99.6934831334186));
#28904=CARTESIAN_POINT('Ctrl Pts',(-0.89583228484855,-16.2806170188525,
99.6947552682589));
#28905=CARTESIAN_POINT('Ctrl Pts',(-0.75438881080454,-16.2560787406678,
99.7270276969224));
#28906=CARTESIAN_POINT('Ctrl Pts',(-0.610348269374357,-16.2370811333547,
99.7521123711276));
#28907=CARTESIAN_POINT('Ctrl Pts',(-0.463368231392308,-16.2240494573673,
99.7693348591778));
#28908=CARTESIAN_POINT('Ctrl Pts',(-0.460459379125149,-16.223791550098,
99.7696757059629));
#28909=CARTESIAN_POINT('Ctrl Pts',(-0.457549716853913,-16.2235360595476,
99.7700133667742));
#28910=CARTESIAN_POINT('Ctrl Pts',(-0.454639273718578,-16.2232829864302,
99.7703478403196));
#28911=CARTESIAN_POINT('Ctrl Pts',(-0.343816465256741,-16.2136465591544,
99.7830838038597));
#28912=CARTESIAN_POINT('Ctrl Pts',(-0.231916920272007,-16.2075215729844,
99.7911914401011));
#28913=CARTESIAN_POINT('Ctrl Pts',(-0.120466936414993,-16.2049482186016,
99.7945991677203));
#28914=CARTESIAN_POINT('Ctrl Pts',(-0.0810973303828984,-16.2040391834926,
99.7958029444208));
#28915=CARTESIAN_POINT('Ctrl Pts',(-0.0417837345711198,-16.2035736224711,
99.7964198693814));
#28916=CARTESIAN_POINT('Ctrl Pts',(-0.002593448913701,-16.2035542480913,
99.7964455441609));
#28917=CARTESIAN_POINT('Ctrl Pts',(-0.00240467522590323,-16.2035541547678,
99.7964456678325));
#28918=CARTESIAN_POINT('Ctrl Pts',(-0.00221590465409573,-16.2035540717971,
99.7964457777851));
#28919=CARTESIAN_POINT('Ctrl Pts',(-0.00202713720613238,-16.2035539991795,
99.7964458740185));
#28920=CARTESIAN_POINT('Ctrl Pts',(0.13576907501567,-16.2035009898142,99.7965161223064));
#28921=CARTESIAN_POINT('Ctrl Pts',(0.273390922467042,-16.2089194398948,
99.7893191842755));
#28922=CARTESIAN_POINT('Ctrl Pts',(0.410216321504649,-16.2196535179823,
99.7751251055922));
#28923=CARTESIAN_POINT('Ctrl Pts',(0.548666154514294,-16.2305150344054,
99.7607625103632));
#28924=CARTESIAN_POINT('Ctrl Pts',(0.686301275430305,-16.2468192467542,
99.7392354386506));
#28925=CARTESIAN_POINT('Ctrl Pts',(0.822466771282481,-16.2684362741424,
99.7107825845366));
#28926=CARTESIAN_POINT('Ctrl Pts',(0.844769907444301,-16.27197702066,99.7061221683605));
#28927=CARTESIAN_POINT('Ctrl Pts',(0.867033578503416,-16.275660368438,99.7012758588322));
#28928=CARTESIAN_POINT('Ctrl Pts',(0.889254858156698,-16.2794858232672,
99.696244607389));
#28929=CARTESIAN_POINT('Ctrl Pts',(0.895235649074151,-16.2805154329861,
99.69489046112));
#28930=CARTESIAN_POINT('Ctrl Pts',(0.901213199410171,-16.2815552972589,
99.6935229664923));
#28931=CARTESIAN_POINT('Ctrl Pts',(0.907187445725223,-16.2826054039495,
99.6921421453941));
#28932=CARTESIAN_POINT('Ctrl Pts',(1.08848423854067,-16.3144723483427,99.650239213483));
#28933=CARTESIAN_POINT('Ctrl Pts',(1.26510257383785,-16.3555152587659,99.596438124243));
#28934=CARTESIAN_POINT('Ctrl Pts',(1.43521884938335,-16.4040633379988,99.5332547185562));
#28935=CARTESIAN_POINT('Ctrl Pts',(1.53332498347954,-16.4320610375491,99.4968168195304));
#28936=CARTESIAN_POINT('Ctrl Pts',(1.62926781977423,-16.4625547855007,99.4572586816574));
#28937=CARTESIAN_POINT('Ctrl Pts',(1.72269009438428,-16.4952228705692,99.4150655759485));
#28938=CARTESIAN_POINT('Ctrl Pts',(1.73223022669911,-16.4985588828353,99.4107568839056));
#28939=CARTESIAN_POINT('Ctrl Pts',(1.74174350750183,-16.5019172867903,99.4064210546897));
#28940=CARTESIAN_POINT('Ctrl Pts',(1.75122967202433,-16.5052977695157,99.4020585662807));
#28941=CARTESIAN_POINT('Ctrl Pts',(1.85503683804843,-16.5422904160884,99.3543198245082));
#28942=CARTESIAN_POINT('Ctrl Pts',(1.95629664396254,-16.5821376767137,99.3031450764253));
#28943=CARTESIAN_POINT('Ctrl Pts',(2.05507188318957,-16.6245975735538,99.2489133667373));
#28944=CARTESIAN_POINT('Ctrl Pts',(2.1592867864,-16.6693957848681,99.191695055546));
#28945=CARTESIAN_POINT('Ctrl Pts',(2.26073646607868,-16.7171028250444,99.1310729372205));
#28946=CARTESIAN_POINT('Ctrl Pts',(2.35945298072967,-16.7674619289491,99.0674634405602));
#28947=CARTESIAN_POINT('Ctrl Pts',(2.39231754695952,-16.7842274125301,99.0462866544548));
#28948=CARTESIAN_POINT('Ctrl Pts',(2.42487881988457,-16.8012870169628,99.0247785979171));
#28949=CARTESIAN_POINT('Ctrl Pts',(2.45713687455928,-16.8186317269496,99.0029542627794));
#28950=CARTESIAN_POINT('Ctrl Pts',(2.53098232469012,-16.8583374044703,98.9529937841238));
#28951=CARTESIAN_POINT('Ctrl Pts',(2.60289021699092,-16.8993427920625,98.9016192560274));
#28952=CARTESIAN_POINT('Ctrl Pts',(2.67301396895445,-16.9415787314616,98.848957107387));
#28953=CARTESIAN_POINT('Ctrl Pts',(2.74686281776279,-16.9860583181297,98.7934974529337));
#28954=CARTESIAN_POINT('Ctrl Pts',(2.81873348542218,-17.031903132171,98.7366089356634));
#28955=CARTESIAN_POINT('Ctrl Pts',(2.88875921131318,-17.0790596222749,98.6784119085654));
#28956=CARTESIAN_POINT('Ctrl Pts',(2.95878493720418,-17.1262161123789,98.6202148814674));
#28957=CARTESIAN_POINT('Ctrl Pts',(3.0269659433531,-17.1746850226114,98.5607082197103));
#28958=CARTESIAN_POINT('Ctrl Pts',(3.09338541157247,-17.2244297295311,98.5000007932762));
#28959=CARTESIAN_POINT('Ctrl Pts',(7.62166314348062,-15.7531022204317,98.500000610284));
#28960=CARTESIAN_POINT('Ctrl Pts',(7.69400225181639,-15.5188970106341,98.6793214334492));
#28961=CARTESIAN_POINT('Ctrl Pts',(7.78580021647469,-15.282866431888,98.8494491913713));
#28962=CARTESIAN_POINT('Ctrl Pts',(8.01090275442513,-14.8162420216974,99.1580199459299));
#28963=CARTESIAN_POINT('Ctrl Pts',(8.14397944499903,-14.5853179903069,99.2969308183713));
#28964=CARTESIAN_POINT('Ctrl Pts',(8.38183223465004,-14.242273311074,99.4748187550338));
#28965=CARTESIAN_POINT('Ctrl Pts',(8.46796561908337,-14.1280782793539,99.5290970577316));
#28966=CARTESIAN_POINT('Ctrl Pts',(8.65039182617701,-13.9063490976389,99.62326558462));
#28967=CARTESIAN_POINT('Ctrl Pts',(8.74705976167071,-13.7981959987251,99.6635148733605));
#28968=CARTESIAN_POINT('Ctrl Pts',(9.05460506897777,-13.4823163139724,99.7618768897716));
#28969=CARTESIAN_POINT('Ctrl Pts',(9.28643675965965,-13.2812823779052,99.7968963262704));
#28970=CARTESIAN_POINT('Ctrl Pts',(9.6503936412052,-13.0174883808938,99.7962149169054));
#28971=CARTESIAN_POINT('Ctrl Pts',(9.775045002922,-12.9350475934176,99.7875063317089));
#28972=CARTESIAN_POINT('Ctrl Pts',(10.0309579794496,-12.7810506313035,99.753358404991));
#28973=CARTESIAN_POINT('Ctrl Pts',(10.1633841214783,-12.708950911147,99.7275975989373));
#28974=CARTESIAN_POINT('Ctrl Pts',(10.5613890038482,-12.5136572830832,99.6277174576398));
#28975=CARTESIAN_POINT('Ctrl Pts',(10.8257011162573,-12.4115301467734,99.5324632749563));
#28976=CARTESIAN_POINT('Ctrl Pts',(11.3534955337226,-12.2529722492584,99.2974531785354));
#28977=CARTESIAN_POINT('Ctrl Pts',(11.6189361780422,-12.1966627203719,99.15615753822));
#28978=CARTESIAN_POINT('Ctrl Pts',(12.1322393649622,-12.1271244860313,98.8472990531187));
#28979=CARTESIAN_POINT('Ctrl Pts',(12.3821304053377,-12.1130390987287,98.6790582739388));
#28980=CARTESIAN_POINT('Ctrl Pts',(12.6268678194693,-12.1166087086112,98.5000000706302));
#28981=CARTESIAN_POINT('Ctrl Pts',(15.4254975876205,-8.26462497236941,98.5000000648311));
#28982=CARTESIAN_POINT('Ctrl Pts',(15.39896159776,-8.18681012723897,98.5601400874524));
#28983=CARTESIAN_POINT('Ctrl Pts',(15.3740814904792,-8.10752087101609,98.6192489818165));
#28984=CARTESIAN_POINT('Ctrl Pts',(15.3509818470288,-8.02689530037569,98.6770789350102));
#28985=CARTESIAN_POINT('Ctrl Pts',(15.3272514958868,-7.94406834651245,98.7364878647956));
#28986=CARTESIAN_POINT('Ctrl Pts',(15.3053993169532,-7.8598303841339,98.7945484303452));
#28987=CARTESIAN_POINT('Ctrl Pts',(15.2855818245971,-7.77428165639307,98.8509939558235));
#28988=CARTESIAN_POINT('Ctrl Pts',(15.2699513231113,-7.70680745269335,98.8955138100007));
#28989=CARTESIAN_POINT('Ctrl Pts',(15.2555868575608,-7.63851671031211,98.9390292514885));
#28990=CARTESIAN_POINT('Ctrl Pts',(15.2425795199653,-7.5694424311712,98.9814016690259));
#28991=CARTESIAN_POINT('Ctrl Pts',(15.2403905735313,-7.55781823091512,98.9885323328984));
#28992=CARTESIAN_POINT('Ctrl Pts',(15.2382391277397,-7.54617292290305,98.9956311576657));
#28993=CARTESIAN_POINT('Ctrl Pts',(15.2361254605807,-7.53450571055501,99.0026979840551));
#28994=CARTESIAN_POINT('Ctrl Pts',(15.2094590945176,-7.38731027626687,99.0918542065011));
#28995=CARTESIAN_POINT('Ctrl Pts',(15.188846331291,-7.23684877733962,99.1757821758146));
#28996=CARTESIAN_POINT('Ctrl Pts',(15.174973938242,-7.08263617831606,99.2535679556245));
#28997=CARTESIAN_POINT('Ctrl Pts',(15.1657087941142,-6.97964010898367,99.305519804054));
#28998=CARTESIAN_POINT('Ctrl Pts',(15.1594497290312,-6.87497109531529,99.3547324640083));
#28999=CARTESIAN_POINT('Ctrl Pts',(15.1563931490129,-6.76848904972109,99.4009428779259));
#29000=CARTESIAN_POINT('Ctrl Pts',(15.1561145921656,-6.75878496779185,99.405154194868));
#29001=CARTESIAN_POINT('Ctrl Pts',(15.1558636606571,-6.74906375936666,99.409340145667));
#29002=CARTESIAN_POINT('Ctrl Pts',(15.1556404821766,-6.73932606051681,99.4135002521259));
#29003=CARTESIAN_POINT('Ctrl Pts',(15.1519973739076,-6.58037036229148,99.4814087628592));
#29004=CARTESIAN_POINT('Ctrl Pts',(15.1557666604135,-6.4169457807656,99.5424448371331));
#29005=CARTESIAN_POINT('Ctrl Pts',(15.1675209018644,-6.25170583458525,99.5945560959231));
#29006=CARTESIAN_POINT('Ctrl Pts',(15.17582303921,-6.1349952213244,99.6313627949797));
#29007=CARTESIAN_POINT('Ctrl Pts',(15.1881085912481,-6.01737791055278,99.663717771867));
#29008=CARTESIAN_POINT('Ctrl Pts',(15.2045787950898,-5.89977535028896,99.6909054353085));
#29009=CARTESIAN_POINT('Ctrl Pts',(15.2053629424752,-5.89417628539394,99.6921998415835));
#29010=CARTESIAN_POINT('Ctrl Pts',(15.2061565022707,-5.88857599398075,99.6934831334187));
#29011=CARTESIAN_POINT('Ctrl Pts',(15.2069595049574,-5.8829744697482,99.694755268259));
#29012=CARTESIAN_POINT('Ctrl Pts',(15.2273306528143,-5.74087098709944,99.7270276969224));
#29013=CARTESIAN_POINT('Ctrl Pts',(15.2537738297661,-5.59800970804934,99.7521123711275));
#29014=CARTESIAN_POINT('Ctrl Pts',(15.2867992989703,-5.45419637581596,99.7693348591779));
#29015=CARTESIAN_POINT('Ctrl Pts',(15.2874528993659,-5.45135019518315,99.7696757059629));
#29016=CARTESIAN_POINT('Ctrl Pts',(15.2881090485028,-5.44850399099787,99.7700133667743));
#29017=CARTESIAN_POINT('Ctrl Pts',(15.2887677380554,-5.44565779119462,99.7703478403196));
#29018=CARTESIAN_POINT('Ctrl Pts',(15.3138490822596,-5.33728121734784,99.7830838038494));
#29019=CARTESIAN_POINT('Ctrl Pts',(15.3426027352871,-5.22896570119097,99.7911914400879));
#29020=CARTESIAN_POINT('Ctrl Pts',(15.3745952688359,-5.12217525765042,99.794599167712));
#29021=CARTESIAN_POINT('Ctrl Pts',(15.3858966024219,-5.0844516299046,99.795802944418));
#29022=CARTESIAN_POINT('Ctrl Pts',(15.3976023968206,-5.04691831207414,99.7964198693814));
#29023=CARTESIAN_POINT('Ctrl Pts',(15.4096944350009,-5.00964014842565,99.7964455441609));
#29024=CARTESIAN_POINT('Ctrl Pts',(15.4097526805226,-5.00946058514123,99.7964456678325));
#29025=CARTESIAN_POINT('Ctrl Pts',(15.4098109349275,-5.00928102801946,99.7964457777851));
#29026=CARTESIAN_POINT('Ctrl Pts',(15.4098691982134,-5.00910147706791,99.7964458740185));
#29027=CARTESIAN_POINT('Ctrl Pts',(15.4524001546504,-4.87803311071218,99.7965161223064));
#29028=CARTESIAN_POINT('Ctrl Pts',(15.5000808965701,-4.74882134906045,99.789319184275));
#29029=CARTESIAN_POINT('Ctrl Pts',(15.5525709850495,-4.62200967425275,99.7751251055903));
#29030=CARTESIAN_POINT('Ctrl Pts',(15.6056842522913,-4.49369245154328,99.7607625103601));
#29031=CARTESIAN_POINT('Ctrl Pts',(15.6637220710776,-4.36783195161589,99.7392354386457));
#29032=CARTESIAN_POINT('Ctrl Pts',(15.7263585381074,-4.24501089831755,99.7107825845292));
#29033=CARTESIAN_POINT('Ctrl Pts',(15.7366180362518,-4.22489350619505,99.7061221683555));
#29034=CARTESIAN_POINT('Ctrl Pts',(15.7470009608666,-4.20485771382844,99.7012758588297));
#29035=CARTESIAN_POINT('Ctrl Pts',(15.7575059376535,-4.18490615157833,99.6962446073893));
#29036=CARTESIAN_POINT('Ctrl Pts',(15.7603333207192,-4.17953624830441,99.6948904611204));
#29037=CARTESIAN_POINT('Ctrl Pts',(15.7631694550505,-4.174172595838,99.6935229664926));
#29038=CARTESIAN_POINT('Ctrl Pts',(15.7660143095013,-4.16881525076341,99.6921421453944));
#29039=CARTESIAN_POINT('Ctrl Pts',(15.8523453647812,-4.00623918165834,99.650239213408));
#29040=CARTESIAN_POINT('Ctrl Pts',(15.9459575594927,-3.85094811953142,99.5964381240503));
#29041=CARTESIAN_POINT('Ctrl Pts',(16.0446983469592,-3.70416010844114,99.5332547182168));
#29042=CARTESIAN_POINT('Ctrl Pts',(16.1016422040798,-3.61950739556519,99.4968168192847));
#29043=CARTESIAN_POINT('Ctrl Pts',(16.1602914485011,-3.53768342251801,99.4572586815263));
#29044=CARTESIAN_POINT('Ctrl Pts',(16.220229714002,-3.45892855318715,99.4150655759483));
#29045=CARTESIAN_POINT('Ctrl Pts',(16.2263505132199,-3.45088623266648,99.4107568839055));
#29046=CARTESIAN_POINT('Ctrl Pts',(16.232484310626,-3.44287636886379,99.4064210546895));
#29047=CARTESIAN_POINT('Ctrl Pts',(16.2386307267991,-3.43489911689133,99.4020585662805));
#29048=CARTESIAN_POINT('Ctrl Pts',(16.3058910028129,-3.34760399166822,99.3543198245105));
#29049=CARTESIAN_POINT('Ctrl Pts',(16.3750790005579,-3.26361367413128,99.3031450764307));
#29050=CARTESIAN_POINT('Ctrl Pts',(16.4459839896695,-3.1827936689224,99.2489133667459));
#29051=CARTESIAN_POINT('Ctrl Pts',(16.5207937966085,-3.09752281475197,99.1916950555618));
#29052=CARTESIAN_POINT('Ctrl Pts',(16.5975155631267,-3.01578072199172,99.1310729372442));
#29053=CARTESIAN_POINT('Ctrl Pts',(16.675914997693,-2.93745755640269,99.0674634405922));
#29054=CARTESIAN_POINT('Ctrl Pts',(16.7020156295919,-2.91138231586673,99.0462866544767));
#29055=CARTESIAN_POINT('Ctrl Pts',(16.7283022642583,-2.88568641274665,99.0247785979286));
#29056=CARTESIAN_POINT('Ctrl Pts',(16.7547663508274,-2.86036698978117,99.0029542627802));
#29057=CARTESIAN_POINT('Ctrl Pts',(16.815348193217,-2.80240552236074,98.9529937841231));
#29058=CARTESIAN_POINT('Ctrl Pts',(16.8765673950423,-2.74668841444027,98.901619256025));
#29059=CARTESIAN_POINT('Ctrl Pts',(16.9384055914977,-2.69304838623452,98.8489571073828));
#29060=CARTESIAN_POINT('Ctrl Pts',(17.0035287415365,-2.6365589055387,98.7934974529301));
#29061=CARTESIAN_POINT('Ctrl Pts',(17.0693390083717,-2.58237266537445,98.7366089356605));
#29062=CARTESIAN_POINT('Ctrl Pts',(17.1358266349136,-2.5303463992957,98.6784119085632));
#29063=CARTESIAN_POINT('Ctrl Pts',(17.2023142614554,-2.47832013321695,98.6202148814659));
#29064=CARTESIAN_POINT('Ctrl Pts',(17.2694800239625,-2.42845385999314,98.5607082197096));
#29065=CARTESIAN_POINT('Ctrl Pts',(17.337314796066,-2.38065715175364,98.5000007932762));
#29066=CARTESIAN_POINT('',(16.,-1.95943487863577E-15,100.));
#29067=CARTESIAN_POINT('Ctrl Pts',(17.3373139553419,2.38065609737472,98.500000610284));
#29068=CARTESIAN_POINT('Ctrl Pts',(17.1369255782473,2.52182806773904,98.6793214334492));
#29069=CARTESIAN_POINT('Ctrl Pts',(16.9408142894144,2.68207058023465,98.8494491913713));
#29070=CARTESIAN_POINT('Ctrl Pts',(16.5665886131438,3.04035068852609,99.1580199459299));
#29071=CARTESIAN_POINT('Ctrl Pts',(16.3880897672633,3.23827359237263,99.2969308183713));
#29072=CARTESIAN_POINT('Ctrl Pts',(16.1353354438601,3.57049167360207,99.4748187550338));
#29073=CARTESIAN_POINT('Ctrl Pts',(16.0533461943871,3.68769759561264,99.5290970577315));
#29074=CARTESIAN_POINT('Ctrl Pts',(15.8988420094756,3.92971331391083,99.62326558462));
#29075=CARTESIAN_POINT('Ctrl Pts',(15.8258543348747,4.05507112943761,99.6635148733605));
#29076=CARTESIAN_POINT('Ctrl Pts',(15.6204716288236,4.44517628877436,99.7618768897715));
#29077=CARTESIAN_POINT('Ctrl Pts',(15.5009169261858,4.72778423157193,99.7968963262704));
#29078=CARTESIAN_POINT('Ctrl Pts',(15.3625027879858,5.15544462350693,99.7962149169054));
#29079=CARTESIAN_POINT('Ctrl Pts',(15.3226163289905,5.29947071769255,99.7875063317089));
#29080=CARTESIAN_POINT('Ctrl Pts',(15.2552379735104,5.59044609999894,99.753358404991));
#29081=CARTESIAN_POINT('Ctrl Pts',(15.2275889932189,5.73867088412122,99.7275975989373));
#29082=CARTESIAN_POINT('Ctrl Pts',(15.1648439881543,6.17754507098126,99.6277174576398));
#29083=CARTESIAN_POINT('Ctrl Pts',(15.14939224423,6.46047984853023,99.5324632749564));
#29084=CARTESIAN_POINT('Ctrl Pts',(15.1616921671213,7.01143925344932,99.2974531785354));
#29085=CARTESIAN_POINT('Ctrl Pts',(15.1901642928368,7.2812889092902,99.15615753822));
#29086=CARTESIAN_POINT('Ctrl Pts',(15.2826489099606,7.7909577462157,98.8472990531188));
#29087=CARTESIAN_POINT('Ctrl Pts',(15.3464734888,8.03297087257739,98.6790582739388));
#29088=CARTESIAN_POINT('Ctrl Pts',(15.4254964096654,8.26462691495157,98.5000000706303));
#29089=CARTESIAN_POINT('Ctrl Pts',(12.6268663212259,12.1166104449801,98.5000000648703));
#29090=CARTESIAN_POINT('Ctrl Pts',(12.5446458775159,12.1154191815706,98.5601503317549));
#29091=CARTESIAN_POINT('Ctrl Pts',(12.4615341179539,12.1162591862567,98.6192693642198));
#29092=CARTESIAN_POINT('Ctrl Pts',(12.3777014366889,12.1192061781927,98.677108972024));
#29093=CARTESIAN_POINT('Ctrl Pts',(12.2915741224031,12.1222338339571,98.736531741335));
#29094=CARTESIAN_POINT('Ctrl Pts',(12.2046849295102,12.1274848184563,98.7946054581518));
#29095=CARTESIAN_POINT('Ctrl Pts',(12.1171781716405,12.1350769190419,98.8510630179462));
#29096=CARTESIAN_POINT('Ctrl Pts',(12.0477278725848,12.1411024383157,98.8958709220112));
#29097=CARTESIAN_POINT('Ctrl Pts',(11.9778875805386,12.1486032210661,98.9396611167267));
#29098=CARTESIAN_POINT('Ctrl Pts',(11.9077182330858,12.1576571523016,98.9822921355009));
#29099=CARTESIAN_POINT('Ctrl Pts',(11.8959551442279,12.1591749403601,98.9894387384001));
#29100=CARTESIAN_POINT('Ctrl Pts',(11.8841835086263,12.1607351471293,98.9965533320493));
#29101=CARTESIAN_POINT('Ctrl Pts',(11.8724026494821,12.1623382885866,99.0036357543384));
#29102=CARTESIAN_POINT('Ctrl Pts',(11.7229964865901,12.1826695064354,99.0934558196869));
#29103=CARTESIAN_POINT('Ctrl Pts',(11.5723364226954,12.2098752719653,99.17796211997));
#29104=CARTESIAN_POINT('Ctrl Pts',(11.4201636564221,12.2447803501146,99.2562190949067));
#29105=CARTESIAN_POINT('Ctrl Pts',(11.3200139902322,12.2677524758806,99.3077224624861));
#29106=CARTESIAN_POINT('Ctrl Pts',(11.2192092247972,12.2940588049852,99.3565196705271));
#29107=CARTESIAN_POINT('Ctrl Pts',(11.1176771661422,12.3239257557741,99.402352828103));
#29108=CARTESIAN_POINT('Ctrl Pts',(11.1083271026094,12.3266761962862,99.4065735928636));
#29109=CARTESIAN_POINT('Ctrl Pts',(11.0989693146526,12.3294584306971,99.4107687371794));
#29110=CARTESIAN_POINT('Ctrl Pts',(11.0896044489173,12.3322723840617,99.4149377803029));
#29111=CARTESIAN_POINT('Ctrl Pts',(10.9368635548845,12.3781679435737,99.4829348442163));
#29112=CARTESIAN_POINT('Ctrl Pts',(10.782180778293,12.4325386244882,99.5439998059348));
#29113=CARTESIAN_POINT('Ctrl Pts',(10.6282589264101,12.4951094361626,99.5960759478411));
#29114=CARTESIAN_POINT('Ctrl Pts',(10.5197442277713,12.5392217742704,99.6327895578719));
#29115=CARTESIAN_POINT('Ctrl Pts',(10.4116066692697,12.5874100607449,99.6650361416488));
#29116=CARTESIAN_POINT('Ctrl Pts',(10.3047803019273,12.6395820517603,99.6921021736601));
#29117=CARTESIAN_POINT('Ctrl Pts',(10.2996691247951,12.6420782546553,99.6933971655926));
#29118=CARTESIAN_POINT('Ctrl Pts',(10.2945597086435,12.6445839057491,99.6946809027462));
#29119=CARTESIAN_POINT('Ctrl Pts',(10.2894520568858,12.6470990367868,99.6959533416378));
#29120=CARTESIAN_POINT('Ctrl Pts',(10.1603732160566,12.7106605743163,99.7281099852292));
#29121=CARTESIAN_POINT('Ctrl Pts',(10.0324732032076,12.780246063646,99.7530425577929));
#29122=CARTESIAN_POINT('Ctrl Pts',(9.9057096702643,12.8564220781232,99.7700686162087));
#29123=CARTESIAN_POINT('Ctrl Pts',(9.78852854272624,12.9268397373706,99.7858076278658));
#29124=CARTESIAN_POINT('Ctrl Pts',(9.67313030478594,13.0025204955551,99.7945520991889));
#29125=CARTESIAN_POINT('Ctrl Pts',(9.56184140661172,13.0818662611236,99.796170916244));
#29126=CARTESIAN_POINT('Ctrl Pts',(9.54796066113928,13.0917628311701,99.796372826658));
#29127=CARTESIAN_POINT('Ctrl Pts',(9.53414386525613,13.1017164514157,99.7964638312962));
#29128=CARTESIAN_POINT('Ctrl Pts',(9.52039555682251,13.1117240463958,99.7964436301271));
#29129=CARTESIAN_POINT('Ctrl Pts',(9.52026709963196,13.1118175522654,99.7964434413777));
#29130=CARTESIAN_POINT('Ctrl Pts',(9.52013864842912,13.1119110628399,99.7964432429205));
#29131=CARTESIAN_POINT('Ctrl Pts',(9.5200102032178,13.1120045781168,99.7964430347553));
#29132=CARTESIAN_POINT('Ctrl Pts',(9.39854187906108,13.2004402920585,99.7962461766987));
#29133=CARTESIAN_POINT('Ctrl Pts',(9.28143127084364,13.2936651206149,99.7875210116457));
#29134=CARTESIAN_POINT('Ctrl Pts',(9.16861451193004,13.3916016257416,99.7704440514027));
#29135=CARTESIAN_POINT('Ctrl Pts',(9.16621596908919,13.3936838066648,99.7700809863659));
#29136=CARTESIAN_POINT('Ctrl Pts',(9.16381939232447,13.3957680959599,99.7697141495905));
#29137=CARTESIAN_POINT('Ctrl Pts',(9.16142477903297,13.3978544944896,99.7693435426229));
#29138=CARTESIAN_POINT('Ctrl Pts',(9.075472786598,13.4727434593481,99.7560410159087));
#29139=CARTESIAN_POINT('Ctrl Pts',(8.9915392884372,13.5509036747022,99.7376874829802));
#29140=CARTESIAN_POINT('Ctrl Pts',(8.91103700497453,13.6308471452239,99.71483060684));
#29141=CARTESIAN_POINT('Ctrl Pts',(8.88817991972763,13.6535455662134,99.7083408335821));
#29142=CARTESIAN_POINT('Ctrl Pts',(8.86559966114202,13.6763878101702,99.7014877883411));
#29143=CARTESIAN_POINT('Ctrl Pts',(8.84332918088663,13.699339853188,99.6942835087751));
#29144=CARTESIAN_POINT('Ctrl Pts',(8.83915122841399,13.7036456671525,99.6929319825717));
#29145=CARTESIAN_POINT('Ctrl Pts',(8.83498423109471,13.7079552668881,99.6915681321738));
#29146=CARTESIAN_POINT('Ctrl Pts',(8.83082841847454,13.7122684141791,99.690192042067));
#29147=CARTESIAN_POINT('Ctrl Pts',(8.69127076550717,13.8571095722995,99.6439811266265));
#29148=CARTESIAN_POINT('Ctrl Pts',(8.56417600488204,14.0055185195395,99.5845379974113));
#29149=CARTESIAN_POINT('Ctrl Pts',(8.44794279484853,14.1572127319379,99.5138249398355));
#29150=CARTESIAN_POINT('Ctrl Pts',(8.3971544618688,14.2234958206366,99.4829267282733));
#29151=CARTESIAN_POINT('Ctrl Pts',(8.34843948385405,14.2904060702255,99.449877297544));
#29152=CARTESIAN_POINT('Ctrl Pts',(8.30166232922778,14.357919515952,99.4148427913138));
#29153=CARTESIAN_POINT('Ctrl Pts',(8.29602633367796,14.3660539457331,99.4106216213264));
#29154=CARTESIAN_POINT('Ctrl Pts',(8.2904184545012,14.3741972107076,99.4063715743575));
#29155=CARTESIAN_POINT('Ctrl Pts',(8.28483845220997,14.3823492736635,99.4020929385903));
#29156=CARTESIAN_POINT('Ctrl Pts',(8.19855951864144,14.5083978416577,99.335935953009));
#29157=CARTESIAN_POINT('Ctrl Pts',(8.118904797062,14.6370031608596,99.2625264797961));
#29158=CARTESIAN_POINT('Ctrl Pts',(8.04618036366085,14.7663488923838,99.1837466668257));
#29159=CARTESIAN_POINT('Ctrl Pts',(7.99257245589043,14.8616944828788,99.1256751116361));
#29160=CARTESIAN_POINT('Ctrl Pts',(7.94273055715436,14.9574417704619,99.0646859940753));
#29161=CARTESIAN_POINT('Ctrl Pts',(7.89678243508475,15.052850115494,99.0015448475647));
#29162=CARTESIAN_POINT('Ctrl Pts',(7.89164895202107,15.0635094656762,98.9944905003654));
#29163=CARTESIAN_POINT('Ctrl Pts',(7.88656339890024,15.074165771925,98.9874085551184));
#29164=CARTESIAN_POINT('Ctrl Pts',(7.8815260287386,15.0848179083459,98.9803001233706));
#29165=CARTESIAN_POINT('Ctrl Pts',(7.82583177602524,15.2025902297611,98.9017077663553));
#29166=CARTESIAN_POINT('Ctrl Pts',(7.7755690708679,15.3204628413966,98.8195805047748));
#29167=CARTESIAN_POINT('Ctrl Pts',(7.73037835310887,15.4384372753898,98.734324448814));
#29168=CARTESIAN_POINT('Ctrl Pts',(7.69023139126286,15.543244530844,98.6585838588093));
#29169=CARTESIAN_POINT('Ctrl Pts',(7.65408652107099,15.6481322437467,98.5803745642654));
#29170=CARTESIAN_POINT('Ctrl Pts',(7.6216630381314,15.7531031392177,98.5000003292224));
#29171=CARTESIAN_POINT('Ctrl Pts',(3.09338453344266,17.2244295663994,98.5000000648311));
#29172=CARTESIAN_POINT('Ctrl Pts',(3.02757828974897,17.1751462307692,98.5601400874492));
#29173=CARTESIAN_POINT('Ctrl Pts',(2.95985810192091,17.1269821149717,98.6192489818104));
#29174=CARTESIAN_POINT('Ctrl Pts',(2.89031680997714,17.0800983770372,98.6770789350014));
#29175=CARTESIAN_POINT('Ctrl Pts',(2.81887677757202,17.0319345356173,98.7364878647822));
#29176=CARTESIAN_POINT('Ctrl Pts',(2.74551440919362,16.9851209165041,98.7945484303274));
#29177=CARTESIAN_POINT('Ctrl Pts',(2.67027667614573,16.9398373505462,98.8509939558017));
#29178=CARTESIAN_POINT('Ctrl Pts',(2.6109349856159,16.9041211846239,98.8955138099865));
#29179=CARTESIAN_POINT('Ctrl Pts',(2.55042549403234,16.8693567660988,98.9390292514817));
#29180=CARTESIAN_POINT('Ctrl Pts',(2.4887514391056,16.8356409267848,98.981401669026));
#29181=CARTESIAN_POINT('Ctrl Pts',(2.47837258935323,16.8299670395897,98.9885323328985));
#29182=CARTESIAN_POINT('Ctrl Pts',(2.46796207659617,16.8243222949697,98.9956311576658));
#29183=CARTESIAN_POINT('Ctrl Pts',(2.45751905733814,16.8187067111523,99.0026979840552));
#29184=CARTESIAN_POINT('Ctrl Pts',(2.3257682405814,16.747859599199,99.0918542065687));
#29185=CARTESIAN_POINT('Ctrl Pts',(2.18904054560583,16.6817605361993,99.1757821759419));
#29186=CARTESIAN_POINT('Ctrl Pts',(2.04666245349801,16.6209127925103,99.2535679558014));
#29187=CARTESIAN_POINT('Ctrl Pts',(1.95157045769963,16.580273581087,99.3055198041657));
#29188=CARTESIAN_POINT('Ctrl Pts',(1.85395846778332,16.5419763524922,99.3547324640608));
#29189=CARTESIAN_POINT('Ctrl Pts',(1.75363255973655,16.5061646105046,99.4009428779258));
#29190=CARTESIAN_POINT('Ctrl Pts',(1.7444895081828,16.5029009609688,99.4051541948679));
#29191=CARTESIAN_POINT('Ctrl Pts',(1.73532163166429,16.4996582923134,99.4093401456669));
#29192=CARTESIAN_POINT('Ctrl Pts',(1.72612949566268,16.4964369225345,99.4135002521257));
#29193=CARTESIAN_POINT('Ctrl Pts',(1.5760794254653,16.4438521085836,99.4814087628433));
#29194=CARTESIAN_POINT('Ctrl Pts',(1.41948863873315,16.3969359400961,99.5424448371047));
#29195=CARTESIAN_POINT('Ctrl Pts',(1.25870385084095,16.3570529365087,99.5945560958869));
#29196=CARTESIAN_POINT('Ctrl Pts',(1.14513996001324,16.3288831753973,99.6313627949585));
#29197=CARTESIAN_POINT('Ctrl Pts',(1.0294828057723,16.3042216818488,99.6637177718581));
#29198=CARTESIAN_POINT('Ctrl Pts',(0.912546551574139,16.2835445868269,99.6909054353086));
#29199=CARTESIAN_POINT('Ctrl Pts',(0.906979209552398,16.2825601491023,99.6921998415835));
#29200=CARTESIAN_POINT('Ctrl Pts',(0.901407792447871,16.2815842840968,99.6934831334187));
#29201=CARTESIAN_POINT('Ctrl Pts',(0.89583228484858,16.2806170188524,99.694755268259));
#29202=CARTESIAN_POINT('Ctrl Pts',(0.754388810804532,16.2560787406678,99.7270276969224));
#29203=CARTESIAN_POINT('Ctrl Pts',(0.610348269374317,16.2370811333546,99.7521123711276));
#29204=CARTESIAN_POINT('Ctrl Pts',(0.463368231392301,16.2240494573673,99.7693348591779));
#29205=CARTESIAN_POINT('Ctrl Pts',(0.460459379125142,16.223791550098,99.7696757059629));
#29206=CARTESIAN_POINT('Ctrl Pts',(0.457549716853904,16.2235360595475,99.7700133667742));
#29207=CARTESIAN_POINT('Ctrl Pts',(0.454639273718568,16.2232829864302,99.7703478403196));
#29208=CARTESIAN_POINT('Ctrl Pts',(0.343816465319919,16.2136465591599,99.7830838038524));
#29209=CARTESIAN_POINT('Ctrl Pts',(0.231916920399598,16.2075215729917,99.7911914400916));
#29210=CARTESIAN_POINT('Ctrl Pts',(0.12046693660562,16.2049482186064,99.7945991677142));
#29211=CARTESIAN_POINT('Ctrl Pts',(0.0810973305097992,16.2040391834944,
99.7958029444185));
#29212=CARTESIAN_POINT('Ctrl Pts',(0.0417837346343648,16.2035736224715,
99.796419869381));
#29213=CARTESIAN_POINT('Ctrl Pts',(0.00259344891369449,16.2035542480916,
99.7964455441606));
#29214=CARTESIAN_POINT('Ctrl Pts',(0.00240467522589664,16.2035541547682,
99.7964456678321));
#29215=CARTESIAN_POINT('Ctrl Pts',(0.00221590465408674,16.2035540717975,
99.7964457777848));
#29216=CARTESIAN_POINT('Ctrl Pts',(0.00202713720612241,16.2035539991798,
99.7964458740181));
#29217=CARTESIAN_POINT('Ctrl Pts',(-0.135769074962828,16.2035009898145,
99.7965161223062));
#29218=CARTESIAN_POINT('Ctrl Pts',(-0.273390922361444,16.2089194398907,
99.789319184281));
#29219=CARTESIAN_POINT('Ctrl Pts',(-0.410216321347207,16.21965351797,99.7751251056086));
#29220=CARTESIAN_POINT('Ctrl Pts',(-0.548666154289857,16.2305150343835,
99.760762510392));
#29221=CARTESIAN_POINT('Ctrl Pts',(-0.686301275139974,16.2468192467176,
99.7392354386988));
#29222=CARTESIAN_POINT('Ctrl Pts',(-0.822466770928219,16.2684362740861,
99.7107825846107));
#29223=CARTESIAN_POINT('Ctrl Pts',(-0.844769907208554,16.2719770206209,
99.7061221684119));
#29224=CARTESIAN_POINT('Ctrl Pts',(-0.86703357838578,16.2756603684177,99.7012758588589));
#29225=CARTESIAN_POINT('Ctrl Pts',(-0.889254858156722,16.2794858232671,
99.6962446073891));
#29226=CARTESIAN_POINT('Ctrl Pts',(-0.895235649074178,16.280515432986,99.6948904611201));
#29227=CARTESIAN_POINT('Ctrl Pts',(-0.901213199410201,16.2815552972589,
99.6935229664924));
#29228=CARTESIAN_POINT('Ctrl Pts',(-0.907187445725255,16.2826054039494,
99.6921421453942));
#29229=CARTESIAN_POINT('Ctrl Pts',(-1.08848423857813,16.3144723483492,99.6502392134744));
#29230=CARTESIAN_POINT('Ctrl Pts',(-1.26510257391078,16.355515258783,99.5964381242207));
#29231=CARTESIAN_POINT('Ctrl Pts',(-1.43521884948873,16.4040633380291,99.5332547185169));
#29232=CARTESIAN_POINT('Ctrl Pts',(-1.53332498354818,16.4320610375712,99.4968168195019));
#29233=CARTESIAN_POINT('Ctrl Pts',(-1.62926781980758,16.4625547855127,99.4572586816421));
#29234=CARTESIAN_POINT('Ctrl Pts',(-1.72269009438418,16.4952228705693,99.4150655759484));
#29235=CARTESIAN_POINT('Ctrl Pts',(-1.73223022669901,16.4985588828354,99.4107568839055));
#29236=CARTESIAN_POINT('Ctrl Pts',(-1.74174350750173,16.5019172867905,99.4064210546896));
#29237=CARTESIAN_POINT('Ctrl Pts',(-1.75122967202423,16.5052977695158,99.4020585662806));
#29238=CARTESIAN_POINT('Ctrl Pts',(-1.85503683804354,16.5422904160868,99.3543198245104));
#29239=CARTESIAN_POINT('Ctrl Pts',(-1.95629664395312,16.58213767671,99.3031450764302));
#29240=CARTESIAN_POINT('Ctrl Pts',(-2.05507188317586,16.6245975735477,99.248913366745));
#29241=CARTESIAN_POINT('Ctrl Pts',(-2.15928678637812,16.669395784858,99.1916950555588));
#29242=CARTESIAN_POINT('Ctrl Pts',(-2.26073646604907,16.71710282503,99.1310729372389));
#29243=CARTESIAN_POINT('Ctrl Pts',(-2.35945298069274,16.7674619289298,99.0674634405845));
#29244=CARTESIAN_POINT('Ctrl Pts',(-2.39231754693524,16.7842274125169,99.0462866544713));
#29245=CARTESIAN_POINT('Ctrl Pts',(-2.4248788198727,16.801287016956,99.0247785979255));
#29246=CARTESIAN_POINT('Ctrl Pts',(-2.45713687455959,16.8186317269493,99.0029542627797));
#29247=CARTESIAN_POINT('Ctrl Pts',(-2.53098232468997,16.8583374044698,98.9529937841244));
#29248=CARTESIAN_POINT('Ctrl Pts',(-2.60289021699031,16.8993427920618,98.9016192560283));
#29249=CARTESIAN_POINT('Ctrl Pts',(-2.67301396895339,16.9415787314606,98.8489571073882));
#29250=CARTESIAN_POINT('Ctrl Pts',(-2.74686281776194,16.9860583181289,98.7934974529346));
#29251=CARTESIAN_POINT('Ctrl Pts',(-2.81873348542151,17.0319031321703,98.7366089356642));
#29252=CARTESIAN_POINT('Ctrl Pts',(-2.88875921131269,17.0790596222744,98.678411908566));
#29253=CARTESIAN_POINT('Ctrl Pts',(-2.95878493720387,17.1262161123785,98.6202148814678));
#29254=CARTESIAN_POINT('Ctrl Pts',(-3.02696594335296,17.1746850226112,98.5607082197105));
#29255=CARTESIAN_POINT('Ctrl Pts',(-3.0933854115725,17.2244297295311,98.5000007932762));
#29256=CARTESIAN_POINT('Origin',(-1.04083408558608E-14,0.,42.));
#29257=CARTESIAN_POINT('',(-11.35,-1.38997411703225E-15,42.));
#29258=CARTESIAN_POINT('Origin',(0.,0.,42.));
#29259=CARTESIAN_POINT('Origin',(0.,0.,0.));
#29260=CARTESIAN_POINT('',(-11.35,-1.38997411703225E-15,0.));
#29261=CARTESIAN_POINT('',(8.09660750783269,7.95408365961204,125.));
#29262=CARTESIAN_POINT('',(5.06279377892661,10.1582783557088,125.));
#29263=CARTESIAN_POINT('Ctrl Pts',(8.09660750783269,7.95408365961205,125.));
#29264=CARTESIAN_POINT('Ctrl Pts',(8.09660750783269,7.95408365961205,124.764102516373));
#29265=CARTESIAN_POINT('Ctrl Pts',(8.06323161817317,7.98850304917249,124.512783030785));
#29266=CARTESIAN_POINT('Ctrl Pts',(7.92569717624602,8.12497441557712,124.050953500858));
#29267=CARTESIAN_POINT('Ctrl Pts',(7.82129658482452,8.22665391752821,123.840405577283));
#29268=CARTESIAN_POINT('Ctrl Pts',(7.5753171261144,8.45370238070912,123.507948276706));
#29269=CARTESIAN_POINT('Ctrl Pts',(7.41718720317046,8.59426386648911,123.363717352429));
#29270=CARTESIAN_POINT('Ctrl Pts',(7.06076432561089,8.88941193496231,123.172231355143));
#29271=CARTESIAN_POINT('Ctrl Pts',(6.86220276900426,9.04368939714487,123.125));
#29272=CARTESIAN_POINT('Ctrl Pts',(6.48052245803477,9.32099637516652,123.125));
#29273=CARTESIAN_POINT('Ctrl Pts',(6.27243697688758,9.46216527979951,123.172231355143));
#29274=CARTESIAN_POINT('Ctrl Pts',(5.88159375674427,9.70993781104404,123.363717352429));
#29275=CARTESIAN_POINT('Ctrl Pts',(5.69904700624421,9.81689241682052,123.507948276706));
#29276=CARTESIAN_POINT('Ctrl Pts',(5.40709925281262,9.98067095023192,123.840405577283));
#29277=CARTESIAN_POINT('Ctrl Pts',(5.27813474293636,10.0485411189259,124.050953500858));
#29278=CARTESIAN_POINT('Ctrl Pts',(5.10584228076216,10.1371721746712,124.512783030785));
#29279=CARTESIAN_POINT('Ctrl Pts',(5.06279377892663,10.1582783557088,124.764102516373));
#29280=CARTESIAN_POINT('Ctrl Pts',(5.06279377892663,10.1582783557088,125.));
#29281=CARTESIAN_POINT('Ctrl Pts',(5.06279377892663,10.1582783557088,125.));
#29282=CARTESIAN_POINT('Ctrl Pts',(5.06279377892663,10.1582783557088,125.235897483627));
#29283=CARTESIAN_POINT('Ctrl Pts',(5.10584228076216,10.1371721746712,125.487216969215));
#29284=CARTESIAN_POINT('Ctrl Pts',(5.27813474293636,10.0485411189259,125.949046499142));
#29285=CARTESIAN_POINT('Ctrl Pts',(5.40709925281262,9.98067095023192,126.159594422717));
#29286=CARTESIAN_POINT('Ctrl Pts',(5.69904700624421,9.81689241682052,126.492051723294));
#29287=CARTESIAN_POINT('Ctrl Pts',(5.88159375674427,9.70993781104404,126.636282647571));
#29288=CARTESIAN_POINT('Ctrl Pts',(6.27243697688758,9.46216527979951,126.827768644857));
#29289=CARTESIAN_POINT('Ctrl Pts',(6.48052245803477,9.32099637516652,126.875));
#29290=CARTESIAN_POINT('Ctrl Pts',(6.86220276900426,9.04368939714487,126.875));
#29291=CARTESIAN_POINT('Ctrl Pts',(7.06076432561089,8.88941193496232,126.827768644857));
#29292=CARTESIAN_POINT('Ctrl Pts',(7.41718720317046,8.59426386648911,126.636282647571));
#29293=CARTESIAN_POINT('Ctrl Pts',(7.5753171261144,8.45370238070912,126.492051723294));
#29294=CARTESIAN_POINT('Ctrl Pts',(7.82129658482452,8.22665391752821,126.159594422717));
#29295=CARTESIAN_POINT('Ctrl Pts',(7.92569717624602,8.12497441557712,125.949046499142));
#29296=CARTESIAN_POINT('Ctrl Pts',(8.06323161817317,7.98850304917249,125.487216969215));
#29297=CARTESIAN_POINT('Ctrl Pts',(8.09660750783269,7.95408365961205,125.235897483627));
#29298=CARTESIAN_POINT('Ctrl Pts',(8.09660750783269,7.95408365961205,125.));
#29299=CARTESIAN_POINT('',(-5.06279377892678,10.1582783557087,125.));
#29300=CARTESIAN_POINT('',(-8.09660750783278,7.95408365961186,125.));
#29301=CARTESIAN_POINT('Ctrl Pts',(-5.06279377892678,10.1582783557087,125.));
#29302=CARTESIAN_POINT('Ctrl Pts',(-5.06279377892679,10.1582783557087,124.764102516373));
#29303=CARTESIAN_POINT('Ctrl Pts',(-5.10584228076231,10.1371721746711,124.512783030785));
#29304=CARTESIAN_POINT('Ctrl Pts',(-5.27813474293652,10.0485411189258,124.050953500858));
#29305=CARTESIAN_POINT('Ctrl Pts',(-5.40709925281278,9.98067095023182,123.840405577283));
#29306=CARTESIAN_POINT('Ctrl Pts',(-5.69904700624437,9.81689241682041,123.507948276706));
#29307=CARTESIAN_POINT('Ctrl Pts',(-5.88159375674444,9.70993781104394,123.363717352429));
#29308=CARTESIAN_POINT('Ctrl Pts',(-6.27243697688773,9.46216527979941,123.172231355143));
#29309=CARTESIAN_POINT('Ctrl Pts',(-6.48052245803492,9.3209963751664,123.125));
#29310=CARTESIAN_POINT('Ctrl Pts',(-6.86220276900441,9.04368939714475,123.125));
#29311=CARTESIAN_POINT('Ctrl Pts',(-7.06076432561104,8.8894119349622,123.172231355143));
#29312=CARTESIAN_POINT('Ctrl Pts',(-7.4171872031706,8.59426386648899,123.363717352429));
#29313=CARTESIAN_POINT('Ctrl Pts',(-7.57531712611454,8.45370238070899,123.507948276706));
#29314=CARTESIAN_POINT('Ctrl Pts',(-7.82129658482466,8.22665391752808,123.840405577283));
#29315=CARTESIAN_POINT('Ctrl Pts',(-7.92569717624616,8.12497441557699,124.050953500858));
#29316=CARTESIAN_POINT('Ctrl Pts',(-8.0632316181733,7.98850304917235,124.512783030785));
#29317=CARTESIAN_POINT('Ctrl Pts',(-8.09660750783282,7.95408365961192,124.764102516373));
#29318=CARTESIAN_POINT('Ctrl Pts',(-8.09660750783282,7.95408365961192,125.));
#29319=CARTESIAN_POINT('Ctrl Pts',(-8.09660750783282,7.95408365961192,125.));
#29320=CARTESIAN_POINT('Ctrl Pts',(-8.09660750783281,7.95408365961192,125.235897483627));
#29321=CARTESIAN_POINT('Ctrl Pts',(-8.0632316181733,7.98850304917235,125.487216969215));
#29322=CARTESIAN_POINT('Ctrl Pts',(-7.92569717624616,8.12497441557699,125.949046499142));
#29323=CARTESIAN_POINT('Ctrl Pts',(-7.82129658482466,8.22665391752808,126.159594422717));
#29324=CARTESIAN_POINT('Ctrl Pts',(-7.57531712611454,8.45370238070899,126.492051723294));
#29325=CARTESIAN_POINT('Ctrl Pts',(-7.4171872031706,8.59426386648899,126.636282647571));
#29326=CARTESIAN_POINT('Ctrl Pts',(-7.06076432561104,8.8894119349622,126.827768644857));
#29327=CARTESIAN_POINT('Ctrl Pts',(-6.86220276900441,9.04368939714475,126.875));
#29328=CARTESIAN_POINT('Ctrl Pts',(-6.48052245803492,9.3209963751664,126.875));
#29329=CARTESIAN_POINT('Ctrl Pts',(-6.27243697688773,9.46216527979941,126.827768644857));
#29330=CARTESIAN_POINT('Ctrl Pts',(-5.88159375674444,9.70993781104394,126.636282647571));
#29331=CARTESIAN_POINT('Ctrl Pts',(-5.69904700624437,9.81689241682041,126.492051723294));
#29332=CARTESIAN_POINT('Ctrl Pts',(-5.40709925281278,9.98067095023182,126.159594422717));
#29333=CARTESIAN_POINT('Ctrl Pts',(-5.27813474293652,10.0485411189258,125.949046499142));
#29334=CARTESIAN_POINT('Ctrl Pts',(-5.10584228076231,10.1371721746711,125.487216969215));
#29335=CARTESIAN_POINT('Ctrl Pts',(-5.06279377892678,10.1582783557087,125.235897483627));
#29336=CARTESIAN_POINT('Ctrl Pts',(-5.06279377892678,10.1582783557087,125.));
#29337=CARTESIAN_POINT('',(-11.2255861412409,-1.67592236860171,125.));
#29338=CARTESIAN_POINT('',(-10.0667724123348,-5.24238430470852,125.));
#29339=CARTESIAN_POINT('Ctrl Pts',(-11.2255861412409,-1.67592236860171,
125.));
#29340=CARTESIAN_POINT('Ctrl Pts',(-11.2255861412409,-1.67592236860171,
124.764102516373));
#29341=CARTESIAN_POINT('Ctrl Pts',(-11.2188156888805,-1.72338609541612,
124.512783030785));
#29342=CARTESIAN_POINT('Ctrl Pts',(-11.1877638445824,-1.91463446673009,
124.050953500858));
#29343=CARTESIAN_POINT('Ctrl Pts',(-11.1630677036069,-2.05826003975628,
123.840405577283));
#29344=CARTESIAN_POINT('Ctrl Pts',(-11.0975218794567,-2.38652920321304,
123.507948276706));
#29345=CARTESIAN_POINT('Ctrl Pts',(-11.0522120528577,-2.59319227061624,
123.363717352429));
#29346=CARTESIAN_POINT('Ctrl Pts',(-10.9373435696191,-3.04147218487716,
123.172231355143));
#29347=CARTESIAN_POINT('Ctrl Pts',(-10.8673859129268,-3.2829968282775,123.125));
#29348=CARTESIAN_POINT('Ctrl Pts',(-10.7215970069731,-3.73168894403405,
123.125));
#29349=CARTESIAN_POINT('Ctrl Pts',(-10.6362293166679,-3.96820656399394,
123.172231355143));
#29350=CARTESIAN_POINT('Ctrl Pts',(-10.4656675492244,-4.39839063326879,
123.363717352429));
#29351=CARTESIAN_POINT('Ctrl Pts',(-10.3808504657421,-4.59221701476649,
123.507948276706));
#29352=CARTESIAN_POINT('Ctrl Pts',(-10.2409263783277,-4.89631921551712,
123.840405577283));
#29353=CARTESIAN_POINT('Ctrl Pts',(-10.1764849823955,-5.02703077237608,
124.050953500858));
#29354=CARTESIAN_POINT('Ctrl Pts',(-10.089193479956,-5.20000577105051,124.512783030785));
#29355=CARTESIAN_POINT('Ctrl Pts',(-10.0667724123348,-5.24238430470852,
124.764102516373));
#29356=CARTESIAN_POINT('Ctrl Pts',(-10.0667724123348,-5.24238430470852,
125.));
#29357=CARTESIAN_POINT('Ctrl Pts',(-10.0667724123348,-5.24238430470852,
125.));
#29358=CARTESIAN_POINT('Ctrl Pts',(-10.0667724123348,-5.24238430470852,
125.235897483627));
#29359=CARTESIAN_POINT('Ctrl Pts',(-10.089193479956,-5.2000057710505,125.487216969215));
#29360=CARTESIAN_POINT('Ctrl Pts',(-10.1764849823955,-5.02703077237607,
125.949046499142));
#29361=CARTESIAN_POINT('Ctrl Pts',(-10.2409263783277,-4.89631921551712,
126.159594422717));
#29362=CARTESIAN_POINT('Ctrl Pts',(-10.3808504657421,-4.59221701476649,
126.492051723294));
#29363=CARTESIAN_POINT('Ctrl Pts',(-10.4656675492244,-4.39839063326879,
126.636282647571));
#29364=CARTESIAN_POINT('Ctrl Pts',(-10.6362293166679,-3.96820656399394,
126.827768644857));
#29365=CARTESIAN_POINT('Ctrl Pts',(-10.7215970069731,-3.73168894403405,
126.875));
#29366=CARTESIAN_POINT('Ctrl Pts',(-10.8673859129268,-3.2829968282775,126.875));
#29367=CARTESIAN_POINT('Ctrl Pts',(-10.9373435696191,-3.04147218487716,
126.827768644857));
#29368=CARTESIAN_POINT('Ctrl Pts',(-11.0522120528577,-2.59319227061624,
126.636282647571));
#29369=CARTESIAN_POINT('Ctrl Pts',(-11.0975218794567,-2.38652920321304,
126.492051723294));
#29370=CARTESIAN_POINT('Ctrl Pts',(-11.1630677036069,-2.05826003975628,
126.159594422717));
#29371=CARTESIAN_POINT('Ctrl Pts',(-11.1877638445824,-1.91463446673009,
125.949046499142));
#29372=CARTESIAN_POINT('Ctrl Pts',(-11.2188156888805,-1.72338609541612,
125.487216969215));
#29373=CARTESIAN_POINT('Ctrl Pts',(-11.2255861412409,-1.67592236860171,
125.235897483627));
#29374=CARTESIAN_POINT('Ctrl Pts',(-11.2255861412409,-1.67592236860171,
125.));
#29375=CARTESIAN_POINT('',(10.0667724123349,-5.24238430470838,125.));
#29376=CARTESIAN_POINT('',(11.2255861412409,-1.67592236860153,125.));
#29377=CARTESIAN_POINT('Ctrl Pts',(10.0667724123349,-5.24238430470838,125.));
#29378=CARTESIAN_POINT('Ctrl Pts',(10.0667724123349,-5.24238430470838,124.764102516373));
#29379=CARTESIAN_POINT('Ctrl Pts',(10.0891934799561,-5.20000577105036,124.512783030785));
#29380=CARTESIAN_POINT('Ctrl Pts',(10.1764849823956,-5.02703077237593,124.050953500858));
#29381=CARTESIAN_POINT('Ctrl Pts',(10.2409263783278,-4.89631921551698,123.840405577283));
#29382=CARTESIAN_POINT('Ctrl Pts',(10.3808504657422,-4.59221701476634,123.507948276706));
#29383=CARTESIAN_POINT('Ctrl Pts',(10.4656675492245,-4.39839063326864,123.363717352429));
#29384=CARTESIAN_POINT('Ctrl Pts',(10.6362293166679,-3.96820656399379,123.172231355143));
#29385=CARTESIAN_POINT('Ctrl Pts',(10.7215970069731,-3.73168894403389,123.125));
#29386=CARTESIAN_POINT('Ctrl Pts',(10.8673859129269,-3.28299682827734,123.125));
#29387=CARTESIAN_POINT('Ctrl Pts',(10.9373435696192,-3.041472184877,123.172231355143));
#29388=CARTESIAN_POINT('Ctrl Pts',(11.0522120528577,-2.59319227061608,123.363717352429));
#29389=CARTESIAN_POINT('Ctrl Pts',(11.0975218794567,-2.38652920321288,123.507948276706));
#29390=CARTESIAN_POINT('Ctrl Pts',(11.163067703607,-2.05826003975611,123.840405577283));
#29391=CARTESIAN_POINT('Ctrl Pts',(11.1877638445825,-1.91463446672993,124.050953500858));
#29392=CARTESIAN_POINT('Ctrl Pts',(11.2188156888806,-1.72338609541595,124.512783030785));
#29393=CARTESIAN_POINT('Ctrl Pts',(11.225586141241,-1.67592236860154,124.764102516373));
#29394=CARTESIAN_POINT('Ctrl Pts',(11.225586141241,-1.67592236860154,125.));
#29395=CARTESIAN_POINT('Ctrl Pts',(11.225586141241,-1.67592236860154,125.));
#29396=CARTESIAN_POINT('Ctrl Pts',(11.225586141241,-1.67592236860154,125.235897483627));
#29397=CARTESIAN_POINT('Ctrl Pts',(11.2188156888806,-1.72338609541595,125.487216969215));
#29398=CARTESIAN_POINT('Ctrl Pts',(11.1877638445825,-1.91463446672993,125.949046499142));
#29399=CARTESIAN_POINT('Ctrl Pts',(11.163067703607,-2.05826003975611,126.159594422717));
#29400=CARTESIAN_POINT('Ctrl Pts',(11.0975218794567,-2.38652920321288,126.492051723294));
#29401=CARTESIAN_POINT('Ctrl Pts',(11.0522120528577,-2.59319227061608,126.636282647571));
#29402=CARTESIAN_POINT('Ctrl Pts',(10.9373435696192,-3.041472184877,126.827768644857));
#29403=CARTESIAN_POINT('Ctrl Pts',(10.8673859129269,-3.28299682827734,126.875));
#29404=CARTESIAN_POINT('Ctrl Pts',(10.7215970069731,-3.73168894403389,126.875));
#29405=CARTESIAN_POINT('Ctrl Pts',(10.6362293166679,-3.96820656399379,126.827768644857));
#29406=CARTESIAN_POINT('Ctrl Pts',(10.4656675492245,-4.39839063326864,126.636282647571));
#29407=CARTESIAN_POINT('Ctrl Pts',(10.3808504657422,-4.59221701476634,126.492051723294));
#29408=CARTESIAN_POINT('Ctrl Pts',(10.2409263783278,-4.89631921551698,126.159594422717));
#29409=CARTESIAN_POINT('Ctrl Pts',(10.1764849823956,-5.02703077237593,125.949046499142));
#29410=CARTESIAN_POINT('Ctrl Pts',(10.0891934799561,-5.20000577105036,125.487216969215));
#29411=CARTESIAN_POINT('Ctrl Pts',(10.0667724123349,-5.24238430470838,125.235897483627));
#29412=CARTESIAN_POINT('Ctrl Pts',(10.0667724123349,-5.24238430470838,125.));
#29413=CARTESIAN_POINT('',(0.,-11.35,126.875));
#29414=CARTESIAN_POINT('',(-4.61755332615425E-16,-11.35,123.125));
#29415=CARTESIAN_POINT('Ctrl Pts',(1.66533453693773E-15,-11.35,126.875));
#29416=CARTESIAN_POINT('Ctrl Pts',(-0.235891405015774,-11.35,126.875));
#29417=CARTESIAN_POINT('Ctrl Pts',(-0.487213095772096,-11.3418984658909,
126.827768644857));
#29418=CARTESIAN_POINT('Ctrl Pts',(-0.949048942792962,-11.3126187736483,
126.636282647571));
#29419=CARTESIAN_POINT('Ctrl Pts',(-1.15959870615561,-11.2918485795503,
126.492051723294));
#29420=CARTESIAN_POINT('Ctrl Pts',(-1.49205600673265,-11.2527456124869,
126.159594422717));
#29421=CARTESIAN_POINT('Ctrl Pts',(-1.63628357112273,-11.2318502953971,
125.949046499142));
#29422=CARTESIAN_POINT('Ctrl Pts',(-1.82776712848652,-11.2022833573772,
125.487216969215));
#29423=CARTESIAN_POINT('Ctrl Pts',(-1.87499999999999,-11.1940553420108,
125.235897483627));
#29424=CARTESIAN_POINT('Ctrl Pts',(-1.87499999999999,-11.1940553420108,
125.));
#29425=CARTESIAN_POINT('Ctrl Pts',(-1.87499999999999,-11.1940553420108,
124.764102516373));
#29426=CARTESIAN_POINT('Ctrl Pts',(-1.82776712848652,-11.2022833573772,
124.512783030785));
#29427=CARTESIAN_POINT('Ctrl Pts',(-1.63628357112274,-11.2318502953971,
124.050953500858));
#29428=CARTESIAN_POINT('Ctrl Pts',(-1.49205600673265,-11.2527456124869,
123.840405577283));
#29429=CARTESIAN_POINT('Ctrl Pts',(-1.15959870615561,-11.2918485795503,
123.507948276706));
#29430=CARTESIAN_POINT('Ctrl Pts',(-0.949048942792962,-11.3126187736483,
123.363717352429));
#29431=CARTESIAN_POINT('Ctrl Pts',(-0.487213095772096,-11.3418984658909,
123.172231355143));
#29432=CARTESIAN_POINT('Ctrl Pts',(-0.235891405015776,-11.35,123.125));
#29433=CARTESIAN_POINT('Ctrl Pts',(-4.85722573273506E-16,-11.35,123.125));
#29434=CARTESIAN_POINT('Ctrl Pts',(1.38777878078145E-16,-11.35,123.125));
#29435=CARTESIAN_POINT('Ctrl Pts',(0.235891405015776,-11.35,123.125));
#29436=CARTESIAN_POINT('Ctrl Pts',(0.487213095772096,-11.3418984658909,
123.172231355143));
#29437=CARTESIAN_POINT('Ctrl Pts',(0.949048942792962,-11.3126187736483,
123.363717352429));
#29438=CARTESIAN_POINT('Ctrl Pts',(1.15959870615561,-11.2918485795503,123.507948276706));
#29439=CARTESIAN_POINT('Ctrl Pts',(1.49205600673265,-11.2527456124869,123.840405577283));
#29440=CARTESIAN_POINT('Ctrl Pts',(1.63628357112274,-11.2318502953971,124.050953500858));
#29441=CARTESIAN_POINT('Ctrl Pts',(1.82776712848652,-11.2022833573772,124.512783030785));
#29442=CARTESIAN_POINT('Ctrl Pts',(1.87499999999999,-11.1940553420108,124.764102516373));
#29443=CARTESIAN_POINT('Ctrl Pts',(1.87499999999999,-11.1940553420108,125.235897483627));
#29444=CARTESIAN_POINT('Ctrl Pts',(1.82776712848652,-11.2022833573772,125.487216969215));
#29445=CARTESIAN_POINT('Ctrl Pts',(1.63628357112274,-11.2318502953971,125.949046499142));
#29446=CARTESIAN_POINT('Ctrl Pts',(1.49205600673265,-11.2527456124869,126.159594422717));
#29447=CARTESIAN_POINT('Ctrl Pts',(1.15959870615561,-11.2918485795503,126.492051723294));
#29448=CARTESIAN_POINT('Ctrl Pts',(0.949048942792963,-11.3126187736483,
126.636282647571));
#29449=CARTESIAN_POINT('Ctrl Pts',(0.487213095772096,-11.3418984658909,
126.827768644857));
#29450=CARTESIAN_POINT('Ctrl Pts',(0.235891405015774,-11.35,126.875));
#29451=CARTESIAN_POINT('Ctrl Pts',(-1.66533453693773E-15,-11.35,126.875));
#29452=CARTESIAN_POINT('Origin',(0.,-106.,125.));
#29453=CARTESIAN_POINT('',(-2.29621274840127E-16,-106.,123.125));
#29454=CARTESIAN_POINT('Origin',(100.811990727286,-32.7558014037442,125.));
#29455=CARTESIAN_POINT('',(101.391397591739,-30.9725704356907,125.));
#29456=CARTESIAN_POINT('Origin',(-100.811990727286,-32.7558014037456,125.));
#29457=CARTESIAN_POINT('',(-100.232583862833,-34.539032371799,125.));
#29458=CARTESIAN_POINT('Origin',(-62.3052367430029,85.7558014037439,125.));
#29459=CARTESIAN_POINT('',(-63.822143607456,84.6537040556955,125.));
#29460=CARTESIAN_POINT('Origin',(62.3052367430017,85.7558014037448,125.));
#29461=CARTESIAN_POINT('',(60.7883298785487,86.8578987517932,125.));
#29462=CARTESIAN_POINT('Origin',(0.,0.,3.75));
#29463=CARTESIAN_POINT('',(15.,-1.83697019872103E-15,2.24999999999999));
#29464=CARTESIAN_POINT('Origin',(0.,0.,2.24999999999999));
#29465=CARTESIAN_POINT('',(15.,-1.83697019872103E-15,3.75));
#29466=CARTESIAN_POINT('Origin',(0.,0.,3.75));
#29467=CARTESIAN_POINT('',(13.5,-1.65327317884892E-15,3.75));
#29468=CARTESIAN_POINT('Origin',(-14.,0.,30.9));
#29469=CARTESIAN_POINT('',(-15.5,-1.8982025386784E-15,30.9));
#29470=CARTESIAN_POINT('Origin',(0.,0.,30.9));
#29471=CARTESIAN_POINT('Origin',(0.,0.,42.));
#29472=CARTESIAN_POINT('',(-15.5,-1.8982025386784E-15,32.8));
#29473=CARTESIAN_POINT('',(-15.5,-1.8982025386784E-15,42.));
#29474=CARTESIAN_POINT('Origin',(0.,0.,32.8));
#29475=CARTESIAN_POINT('Origin',(-14.,0.,32.8));
#29476=CARTESIAN_POINT('Origin',(-12.2482946431511,16.8583313034371,100.));
#29477=CARTESIAN_POINT('',(-8.00253786203375,15.4036548382545,98.2928932187211));
#29478=CARTESIAN_POINT('',(-8.00253786221767,15.4036548377177,0.5));
#29479=CARTESIAN_POINT('',(-8.00253786221767,15.4036548377177,100.));
#29480=CARTESIAN_POINT('',(-12.1768261106186,12.3708569011015,0.5));
#29481=CARTESIAN_POINT('Origin',(-12.2482946431511,16.8583313034371,0.5));
#29482=CARTESIAN_POINT('',(-12.1768414139071,12.3708281240615,98.2929155812438));
#29483=CARTESIAN_POINT('',(-12.1768261106186,12.3708569011015,100.));
#29484=CARTESIAN_POINT('Ctrl Pts',(-12.1768223332082,12.3708569612629,98.2928961772889));
#29485=CARTESIAN_POINT('Ctrl Pts',(-11.9766556305925,12.3740450279548,98.4496670611162));
#29486=CARTESIAN_POINT('Ctrl Pts',(-11.7718386279247,12.390541715911,98.5976778122645));
#29487=CARTESIAN_POINT('Ctrl Pts',(-11.3497031910366,12.455981009676,98.870667594539));
#29488=CARTESIAN_POINT('Ctrl Pts',(-11.1323782772714,12.5051975008586,98.9953666813421));
#29489=CARTESIAN_POINT('Ctrl Pts',(-10.6948166070868,12.6414901598492,99.2055148722619));
#29490=CARTESIAN_POINT('Ctrl Pts',(-10.4709805367995,12.7297564325018,99.2925877229868));
#29491=CARTESIAN_POINT('Ctrl Pts',(-10.0271356237447,12.9505917384117,99.4120512183375));
#29492=CARTESIAN_POINT('Ctrl Pts',(-9.8121776999094,13.0805177296113,99.4431642901975));
#29493=CARTESIAN_POINT('Ctrl Pts',(-9.40304146226852,13.3782342507087,99.4426185746832));
#29494=CARTESIAN_POINT('Ctrl Pts',(-9.20848272501231,13.5474714192234,99.4095817567495));
#29495=CARTESIAN_POINT('Ctrl Pts',(-8.86697618306585,13.8970925183944,99.2902945556315));
#29496=CARTESIAN_POINT('Ctrl Pts',(-8.71497133569482,14.081422575003,99.2037727159813));
#29497=CARTESIAN_POINT('Ctrl Pts',(-8.44923508864959,14.4577600834109,98.9917454068753));
#29498=CARTESIAN_POINT('Ctrl Pts',(-8.33757587869828,14.6461685366907,98.8686812585125));
#29499=CARTESIAN_POINT('Ctrl Pts',(-8.14664284052531,15.024254464469,98.5978506351621));
#29500=CARTESIAN_POINT('Ctrl Pts',(-8.0672915044469,15.2146587124184,98.4493425737989));
#29501=CARTESIAN_POINT('Ctrl Pts',(-8.00253786221767,15.4036548377177,98.2928932188135));
#29502=CARTESIAN_POINT('Origin',(-19.8181570368417,6.43930956430665,100.));
#29503=CARTESIAN_POINT('',(-15.5282646243346,7.75803424826111,98.292893216895));
#29504=CARTESIAN_POINT('',(-15.5282302736771,7.75804480287585,0.5));
#29505=CARTESIAN_POINT('',(-15.5282302736771,7.75804480287585,100.));
#29506=CARTESIAN_POINT('',(-17.122666505727,2.85087466042015,0.5));
#29507=CARTESIAN_POINT('Origin',(-19.8181570368417,6.43930956430665,0.5));
#29508=CARTESIAN_POINT('',(-17.1226921163487,2.85090171197058,98.2928992166646));
#29509=CARTESIAN_POINT('',(-17.122666505727,2.85087466042014,100.));
#29510=CARTESIAN_POINT('Ctrl Pts',(-17.1226921163487,2.85090171197058,98.2928992166646));
#29511=CARTESIAN_POINT('Ctrl Pts',(-17.0341768248206,2.91742750076187,98.3796187467357));
#29512=CARTESIAN_POINT('Ctrl Pts',(-16.9465325507274,2.98842601539338,98.4639979993741));
#29513=CARTESIAN_POINT('Ctrl Pts',(-16.8602662415713,3.06403584549534,98.5451592717705));
#29514=CARTESIAN_POINT('Ctrl Pts',(-16.779093354132,3.13518144437646,98.621528539137));
#29515=CARTESIAN_POINT('Ctrl Pts',(-16.6991399085188,3.21041016146199,98.6950495057339));
#29516=CARTESIAN_POINT('Ctrl Pts',(-16.6208399982642,3.28987088086897,98.7649644149981));
#29517=CARTESIAN_POINT('Ctrl Pts',(-16.5483443892419,3.36344124931553,98.8296965955378));
#29518=CARTESIAN_POINT('Ctrl Pts',(-16.4772659522328,3.44063971604016,98.8913379369445));
#29519=CARTESIAN_POINT('Ctrl Pts',(-16.4079655937323,3.52161023732575,98.94925502686));
#29520=CARTESIAN_POINT('Ctrl Pts',(-16.3667264774378,3.56979401033893,98.9837202108525));
#29521=CARTESIAN_POINT('Ctrl Pts',(-16.3261173458799,3.6193140120376,99.0168659278914));
#29522=CARTESIAN_POINT('Ctrl Pts',(-16.2862179546654,3.67020490800035,99.0485518299931));
#29523=CARTESIAN_POINT('Ctrl Pts',(-16.264008084157,3.69853316502344,99.0661896876446));
#29524=CARTESIAN_POINT('Ctrl Pts',(-16.2419673252237,3.72735801914113,99.0834087225827));
#29525=CARTESIAN_POINT('Ctrl Pts',(-16.2201221063559,3.75667052759835,99.1001725241583));
#29526=CARTESIAN_POINT('Ctrl Pts',(-16.1531828850613,3.84649139422363,99.1515410103338));
#29527=CARTESIAN_POINT('Ctrl Pts',(-16.0879525207372,3.94106193303834,99.1987035934502));
#29528=CARTESIAN_POINT('Ctrl Pts',(-16.0253317064903,4.04003035297009,99.2404898931802));
#29529=CARTESIAN_POINT('Ctrl Pts',(-15.9694771336334,4.12830513649192,99.2777611415784));
#29530=CARTESIAN_POINT('Ctrl Pts',(-15.9156991936721,4.22007811560318,99.3107542880724));
#29531=CARTESIAN_POINT('Ctrl Pts',(-15.8646538658275,4.3150810117854,99.338614700467));
#29532=CARTESIAN_POINT('Ctrl Pts',(-15.8558170201725,4.33152768704031,99.3434378287456));
#29533=CARTESIAN_POINT('Ctrl Pts',(-15.8470709517408,4.34805391388866,99.3481021122734));
#29534=CARTESIAN_POINT('Ctrl Pts',(-15.8384173641326,4.36465767345712,99.3526059457037));
#29535=CARTESIAN_POINT('Ctrl Pts',(-15.791242699382,4.45517236247468,99.3771584020708));
#29536=CARTESIAN_POINT('Ctrl Pts',(-15.7470132255795,4.54760825118705,99.3968131856348));
#29537=CARTESIAN_POINT('Ctrl Pts',(-15.7058800813114,4.64171660717791,99.4114442249333));
#29538=CARTESIAN_POINT('Ctrl Pts',(-15.6654834850893,4.73413981784503,99.4258132744522));
#29539=CARTESIAN_POINT('Ctrl Pts',(-15.6280730601102,4.82817661116081,99.4353369845748));
#29540=CARTESIAN_POINT('Ctrl Pts',(-15.5938154741567,4.92360774400562,99.4398549403144));
#29541=CARTESIAN_POINT('Ctrl Pts',(-15.5782983430131,4.96683371461404,99.4419013691495));
#29542=CARTESIAN_POINT('Ctrl Pts',(-15.5634284197273,5.01034594078258,99.4429202057471));
#29543=CARTESIAN_POINT('Ctrl Pts',(-15.54922304886,5.05412478637214,99.4428936080771));
#29544=CARTESIAN_POINT('Ctrl Pts',(-15.5490927096604,5.05452647244875,99.4428933640342));
#29545=CARTESIAN_POINT('Ctrl Pts',(-15.5489624219417,5.054928196245,99.4428930314822));
#29546=CARTESIAN_POINT('Ctrl Pts',(-15.5488321857355,5.05532995765703,99.4428926104257));
#29547=CARTESIAN_POINT('Ctrl Pts',(-15.520558415848,5.14255078544335,99.4428012007084));
#29548=CARTESIAN_POINT('Ctrl Pts',(-15.4947275500994,5.23150600734416,99.4385281272485));
#29549=CARTESIAN_POINT('Ctrl Pts',(-15.471706829825,5.32092879229154,99.4301496922843));
#29550=CARTESIAN_POINT('Ctrl Pts',(-15.4609854482667,5.36257543870359,99.4262476250579));
#29551=CARTESIAN_POINT('Ctrl Pts',(-15.450873222712,5.40432327523601,99.4214557128978));
#29552=CARTESIAN_POINT('Ctrl Pts',(-15.4414050589843,5.44604404739281,99.4157848279575));
#29553=CARTESIAN_POINT('Ctrl Pts',(-15.4199748253035,5.5404748073983,99.4029493518352));
#29554=CARTESIAN_POINT('Ctrl Pts',(-15.4018814394618,5.63432924109033,99.3857576708392));
#29555=CARTESIAN_POINT('Ctrl Pts',(-15.3869155759318,5.72751309909371,99.3645857641554));
#29556=CARTESIAN_POINT('Ctrl Pts',(-15.3837402684824,5.74728391939332,99.3600937204537));
#29557=CARTESIAN_POINT('Ctrl Pts',(-15.3807056347888,5.7670245688614,99.3554226501144));
#29558=CARTESIAN_POINT('Ctrl Pts',(-15.3778094961913,5.78673417175796,99.3505763727328));
#29559=CARTESIAN_POINT('Ctrl Pts',(-15.3752577835933,5.80409979164075,99.346306443435));
#29560=CARTESIAN_POINT('Ctrl Pts',(-15.3728123902272,5.82144944475451,99.3418984809087));
#29561=CARTESIAN_POINT('Ctrl Pts',(-15.3704721534173,5.83878192917335,99.3373550074188));
#29562=CARTESIAN_POINT('Ctrl Pts',(-15.3593482394804,5.92116891845956,99.3157583861446));
#29563=CARTESIAN_POINT('Ctrl Pts',(-15.3506235797195,6.00347700634779,99.2909304823459));
#29564=CARTESIAN_POINT('Ctrl Pts',(-15.3441858677526,6.0851481288972,99.2633292101836));
#29565=CARTESIAN_POINT('Ctrl Pts',(-15.3425499146296,6.10590241686122,99.2563151673647));
#29566=CARTESIAN_POINT('Ctrl Pts',(-15.3410614816306,6.12661564803922,99.2491222220216));
#29567=CARTESIAN_POINT('Ctrl Pts',(-15.3397184006096,6.14727885378191,99.2417582529879));
#29568=CARTESIAN_POINT('Ctrl Pts',(-15.3327242044555,6.2548840629056,99.2034098264312));
#29569=CARTESIAN_POINT('Ctrl Pts',(-15.3296610105928,6.36126591155503,99.160338318682));
#29570=CARTESIAN_POINT('Ctrl Pts',(-15.3302281887388,6.46556449283516,99.1134130969483));
#29571=CARTESIAN_POINT('Ctrl Pts',(-15.3302886839739,6.47668898208729,99.1084080516407));
#29572=CARTESIAN_POINT('Ctrl Pts',(-15.3303904984979,6.48778978667583,99.1033591232898));
#29573=CARTESIAN_POINT('Ctrl Pts',(-15.33053328063,6.49886587344165,99.0982673376955));
#29574=CARTESIAN_POINT('Ctrl Pts',(-15.3309963783101,6.53478990686087,99.0817527075989));
#29575=CARTESIAN_POINT('Ctrl Pts',(-15.3318903061923,6.57044546362381,99.0647972731996));
#29576=CARTESIAN_POINT('Ctrl Pts',(-15.3332026482509,6.60579801928923,99.0474373027683));
#29577=CARTESIAN_POINT('Ctrl Pts',(-15.3375368438073,6.72255484245913,98.990103541185));
#29578=CARTESIAN_POINT('Ctrl Pts',(-15.3462629212699,6.83634522428608,98.9284409581762));
#29579=CARTESIAN_POINT('Ctrl Pts',(-15.3589352465123,6.94755494288783,98.8630104837108));
#29580=CARTESIAN_POINT('Ctrl Pts',(-15.3669751681725,7.01811164091287,98.8214983003645));
#29581=CARTESIAN_POINT('Ctrl Pts',(-15.3766042177857,7.08762906317595,98.7784686514901));
#29582=CARTESIAN_POINT('Ctrl Pts',(-15.3877148061349,7.15620112277753,98.7340573318784));
#29583=CARTESIAN_POINT('Ctrl Pts',(-15.3963658244922,7.20959326797821,98.6994774222324));
#29584=CARTESIAN_POINT('Ctrl Pts',(-15.4059126278986,7.2623986669834,98.6640680699513));
#29585=CARTESIAN_POINT('Ctrl Pts',(-15.4163108690968,7.31468638761787,98.6278739858463));
#29586=CARTESIAN_POINT('Ctrl Pts',(-15.434289247329,7.40509094744193,98.5652950437535));
#29587=CARTESIAN_POINT('Ctrl Pts',(-15.4548766711216,7.49387327036431,98.500330324093));
#29588=CARTESIAN_POINT('Ctrl Pts',(-15.477753267434,7.58081992020101,98.4335380215097));
#29589=CARTESIAN_POINT('Ctrl Pts',(-15.4935322900588,7.64079095506091,98.3874683510381));
#29590=CARTESIAN_POINT('Ctrl Pts',(-15.5104013233047,7.69988835331403,98.3405281737054));
#29591=CARTESIAN_POINT('Ctrl Pts',(-15.5282646243346,7.75803424826111,98.292893216895));
#29592=CARTESIAN_POINT('Origin',(-19.8181570368417,-6.43930956430665,100.));
#29593=CARTESIAN_POINT('',(-17.1226665061807,-2.85087466007935,98.2928932187212));
#29594=CARTESIAN_POINT('',(-17.122666505727,-2.85087466042014,0.5));
#29595=CARTESIAN_POINT('',(-17.122666505727,-2.85087466042014,100.));
#29596=CARTESIAN_POINT('',(-15.5282302736771,-7.75804480287584,0.5));
#29597=CARTESIAN_POINT('Origin',(-19.8181570368417,-6.43930956430665,0.5));
#29598=CARTESIAN_POINT('',(-15.5282076340618,-7.7580682497622,98.2929155812433));
#29599=CARTESIAN_POINT('',(-15.5282302736771,-7.75804480287584,100.));
#29600=CARTESIAN_POINT('Ctrl Pts',(-15.5282291636101,-7.7580411917542,98.2928961772888));
#29601=CARTESIAN_POINT('Ctrl Pts',(-15.4694062823956,-7.56668617809925,
98.4496670611161));
#29602=CARTESIAN_POINT('Ctrl Pts',(-15.4218036304123,-7.36679587613455,
98.5976778122644));
#29603=CARTESIAN_POINT('Ctrl Pts',(-15.3535930732429,-6.94509936424973,
98.870667594539));
#29604=CARTESIAN_POINT('Ctrl Pts',(-15.3332436462368,-6.72320235668113,
98.9953666813422));
#29605=CARTESIAN_POINT('Ctrl Pts',(-15.3276516755189,-6.26493973113449,
99.2055148722619));
#29606=CARTESIAN_POINT('Ctrl Pts',(-15.3424287396213,-6.02478319962601,
99.2925877229868));
#29607=CARTESIAN_POINT('Ctrl Pts',(-15.4152999753342,-5.5344197403566,99.4120512183375));
#29608=CARTESIAN_POINT('Ctrl Pts',(-15.47244128436,-5.28983326687213,99.4431642901975));
#29609=CARTESIAN_POINT('Ctrl Pts',(-15.6291564713127,-4.80872211748601,
99.4426185746832));
#29610=CARTESIAN_POINT('Ctrl Pts',(-15.7299886270117,-4.5713886014654,99.4095817567495));
#29611=CARTESIAN_POINT('Ctrl Pts',(-15.9569667264609,-4.13855771815389,
99.2902945556315));
#29612=CARTESIAN_POINT('Ctrl Pts',(-16.0853029468825,-3.93703139748708,
99.2037727159813));
#29613=CARTESIAN_POINT('Ctrl Pts',(-16.3611041702218,-3.56800652240012,
98.9917454068753));
#29614=CARTESIAN_POINT('Ctrl Pts',(-16.5057866639851,-3.40359088922422,
98.8686812585125));
#29615=CARTESIAN_POINT('Ctrl Pts',(-16.8063661957351,-3.10516780207624,
98.5978506351621));
#29616=CARTESIAN_POINT('Ctrl Pts',(-16.9629304851031,-2.97086204840461,
98.4493425737989));
#29617=CARTESIAN_POINT('Ctrl Pts',(-17.122666505727,-2.85087466042014,98.2928932188135));
#29618=CARTESIAN_POINT('Origin',(-12.2482946431511,-16.8583313034371,100.));
#29619=CARTESIAN_POINT('',(-12.1768261122223,-12.3708569010759,98.2928932196637));
#29620=CARTESIAN_POINT('',(-12.1768261106186,-12.3708569011015,0.5));
#29621=CARTESIAN_POINT('',(-12.1768261106186,-12.3708569011015,100.));
#29622=CARTESIAN_POINT('',(-8.00253786221767,-15.4036548377177,0.5));
#29623=CARTESIAN_POINT('Origin',(-12.2482946431511,-16.8583313034371,0.5));
#29624=CARTESIAN_POINT('',(-8.00250696667693,-15.403660603589,98.2929148412897));
#29625=CARTESIAN_POINT('',(-8.00253786221767,-15.4036548377177,100.));
#29626=CARTESIAN_POINT('Ctrl Pts',(-8.00250708598546,-15.403660255427,98.2929146461939));
#29627=CARTESIAN_POINT('Ctrl Pts',(-8.04095434018313,-15.2913939276981,
98.3858632379294));
#29628=CARTESIAN_POINT('Ctrl Pts',(-8.08445379524241,-15.1789643815613,
98.4757075594532));
#29629=CARTESIAN_POINT('Ctrl Pts',(-8.13349045375881,-15.0664065104411,
98.5618687048014));
#29630=CARTESIAN_POINT('Ctrl Pts',(-8.14594002061682,-15.0378299967817,
98.5837435423622));
#29631=CARTESIAN_POINT('Ctrl Pts',(-8.15874627806111,-15.0092451974238,
98.6053811116416));
#29632=CARTESIAN_POINT('Ctrl Pts',(-8.17191669602579,-14.9806526573416,
98.6267722404462));
#29633=CARTESIAN_POINT('Ctrl Pts',(-8.19442659046237,-14.9317844239531,
98.6633323596894));
#29634=CARTESIAN_POINT('Ctrl Pts',(-8.21808777573002,-14.8827759730826,
98.6992365502331));
#29635=CARTESIAN_POINT('Ctrl Pts',(-8.24287820376329,-14.8337655789499,
98.7343285177238));
#29636=CARTESIAN_POINT('Ctrl Pts',(-8.29540418082449,-14.7299223199906,
98.8086814041273));
#29637=CARTESIAN_POINT('Ctrl Pts',(-8.35322906336708,-14.6256182642626,
98.8796681588562));
#29638=CARTESIAN_POINT('Ctrl Pts',(-8.41624979625317,-14.522181993344,98.9457243517455));
#29639=CARTESIAN_POINT('Ctrl Pts',(-8.45042299052846,-14.4660933441116,
98.9815435339307));
#29640=CARTESIAN_POINT('Ctrl Pts',(-8.48612332307116,-14.4102605388657,
99.015912405446));
#29641=CARTESIAN_POINT('Ctrl Pts',(-8.5233300376651,-14.3548990672715,99.0485791162112));
#29642=CARTESIAN_POINT('Ctrl Pts',(-8.54347127793551,-14.3249300492255,
99.0662627004123));
#29643=CARTESIAN_POINT('Ctrl Pts',(-8.56405612172788,-14.2950703500544,
99.0834771132439));
#29644=CARTESIAN_POINT('Ctrl Pts',(-8.58510094647072,-14.2653257640176,
99.1001978976778));
#29645=CARTESIAN_POINT('Ctrl Pts',(-8.64085775874582,-14.1865195339767,
99.1444984632641));
#29646=CARTESIAN_POINT('Ctrl Pts',(-8.69986277604752,-14.1084893186481,
99.1853565450778));
#29647=CARTESIAN_POINT('Ctrl Pts',(-8.76251977964325,-14.0312399826521,
99.2223453246317));
#29648=CARTESIAN_POINT('Ctrl Pts',(-8.82234975489544,-13.9574760680751,
99.2576652033095));
#29649=CARTESIAN_POINT('Ctrl Pts',(-8.88550949801275,-13.8844241448053,
99.2894572254271));
#29650=CARTESIAN_POINT('Ctrl Pts',(-8.95238110253115,-13.8120961796839,
99.3173134272134));
#29651=CARTESIAN_POINT('Ctrl Pts',(-8.96841979764084,-13.7947488139546,
99.3239945459122));
#29652=CARTESIAN_POINT('Ctrl Pts',(-8.98467216422782,-13.7774431305777,
99.3304490804178));
#29653=CARTESIAN_POINT('Ctrl Pts',(-9.00114376230899,-13.7601793662716,
99.3366710553149));
#29654=CARTESIAN_POINT('Ctrl Pts',(-9.01384496169299,-13.7468673299111,
99.3414688013102));
#29655=CARTESIAN_POINT('Ctrl Pts',(-9.02667804656013,-13.7335844186059,
99.346122084825));
#29656=CARTESIAN_POINT('Ctrl Pts',(-9.03963548955908,-13.7203394312888,
99.350626662246));
#29657=CARTESIAN_POINT('Ctrl Pts',(-9.11972744908156,-13.6384701158562,
99.378470152084));
#29658=CARTESIAN_POINT('Ctrl Pts',(-9.20426990945249,-13.5583572449624,
99.4004995600324));
#29659=CARTESIAN_POINT('Ctrl Pts',(-9.29128918150773,-13.4821421839037,
99.4158205242222));
#29660=CARTESIAN_POINT('Ctrl Pts',(-9.39222822782236,-13.39373561147,99.4335922600391));
#29661=CARTESIAN_POINT('Ctrl Pts',(-9.49729440462544,-13.3096962059213,
99.4426890000595));
#29662=CARTESIAN_POINT('Ctrl Pts',(-9.6065927128656,-13.2301161534923,99.4428904203957));
#29663=CARTESIAN_POINT('Ctrl Pts',(-9.60682851186603,-13.2299444683389,
99.4428908549378));
#29664=CARTESIAN_POINT('Ctrl Pts',(-9.60706433486258,-13.2297728014511,
99.4428912473282));
#29665=CARTESIAN_POINT('Ctrl Pts',(-9.60730018182524,-13.2296011528498,
99.4428915975688));
#29666=CARTESIAN_POINT('Ctrl Pts',(-9.68141111896221,-13.1756634698788,
99.443001654775));
#29667=CARTESIAN_POINT('Ctrl Pts',(-9.7579136919251,-13.1235161930304,99.4389375211795));
#29668=CARTESIAN_POINT('Ctrl Pts',(-9.83576642333202,-13.0738739727025,
99.4307630339894));
#29669=CARTESIAN_POINT('Ctrl Pts',(-9.87237363861166,-13.0505316517119,
99.4269192997111));
#29670=CARTESIAN_POINT('Ctrl Pts',(-9.90927903493427,-13.0277429117627,
99.4221673968399));
#29671=CARTESIAN_POINT('Ctrl Pts',(-9.94637331208393,-13.005580020478,99.4165172327954));
#29672=CARTESIAN_POINT('Ctrl Pts',(-10.0295053402403,-12.9559107387482,
99.4038546435089));
#29673=CARTESIAN_POINT('Ctrl Pts',(-10.113122012639,-12.9095945146346,99.386832149816));
#29674=CARTESIAN_POINT('Ctrl Pts',(-10.1970690548685,-12.8664609300821,
99.3658258363157));
#29675=CARTESIAN_POINT('Ctrl Pts',(-10.2150684963089,-12.857212475239,99.3613217835261));
#29676=CARTESIAN_POINT('Ctrl Pts',(-10.2330831050167,-12.8481102206571,
99.3566347314641));
#29677=CARTESIAN_POINT('Ctrl Pts',(-10.2511113268446,-12.8391523023418,
99.3517686237608));
#29678=CARTESIAN_POINT('Ctrl Pts',(-10.2669187778883,-12.8312978474447,
99.347501937893));
#29679=CARTESIAN_POINT('Ctrl Pts',(-10.282743992679,-12.8235507352674,99.3430956262505));
#29680=CARTESIAN_POINT('Ctrl Pts',(-10.2985854655186,-12.8159101990171,
99.3385522499821));
#29681=CARTESIAN_POINT('Ctrl Pts',(-10.373846061876,-12.7796110922031,99.3169673120849));
#29682=CARTESIAN_POINT('Ctrl Pts',(-10.4497789727234,-12.7456422248302,
99.2921178033657));
#29683=CARTESIAN_POINT('Ctrl Pts',(-10.5258154871132,-12.7140687420283,
99.2644650244212));
#29684=CARTESIAN_POINT('Ctrl Pts',(-10.5448521425387,-12.7061639410586,
99.2575418187937));
#29685=CARTESIAN_POINT('Ctrl Pts',(-10.5638953135564,-12.6984091102452,
99.2504430888631));
#29686=CARTESIAN_POINT('Ctrl Pts',(-10.5829361512679,-12.6908049207666,
99.2431764205676));
#29687=CARTESIAN_POINT('Ctrl Pts',(-10.6820892557964,-12.6512069258858,
99.2053360307699));
#29688=CARTESIAN_POINT('Ctrl Pts',(-10.7813009536874,-12.6156428244173,
99.1628582909476));
#29689=CARTESIAN_POINT('Ctrl Pts',(-10.8797010333698,-12.5840907770436,
99.1165798460778));
#29690=CARTESIAN_POINT('Ctrl Pts',(-10.891559547104,-12.5802883371642,99.1110026801257));
#29691=CARTESIAN_POINT('Ctrl Pts',(-10.9034062978763,-12.5765441851341,
99.1053702615889));
#29692=CARTESIAN_POINT('Ctrl Pts',(-10.9152397813687,-12.5728582981514,
99.0996840124349));
#29693=CARTESIAN_POINT('Ctrl Pts',(-10.9496077250953,-12.5621533897882,
99.0831694593816));
#29694=CARTESIAN_POINT('Ctrl Pts',(-10.9838534531502,-12.5519431297429,
99.0662118234554));
#29695=CARTESIAN_POINT('Ctrl Pts',(-11.0179405472129,-12.5422262222296,
99.0488473569643));
#29696=CARTESIAN_POINT('Ctrl Pts',(-11.1286979038751,-12.5106535986106,
98.9924259323376));
#29697=CARTESIAN_POINT('Ctrl Pts',(-11.2380248634249,-12.484033807446,98.9317993629228));
#29698=CARTESIAN_POINT('Ctrl Pts',(-11.3461476368695,-12.4618433879349,
98.8675030974997));
#29699=CARTESIAN_POINT('Ctrl Pts',(-11.4178105090686,-12.4471357630118,
98.824888069184));
#29700=CARTESIAN_POINT('Ctrl Pts',(-11.4889441178986,-12.4343747574801,
98.7806601364314));
#29701=CARTESIAN_POINT('Ctrl Pts',(-11.5596115261684,-12.4234165163235,
98.7349665698175));
#29702=CARTESIAN_POINT('Ctrl Pts',(-11.6130987298848,-12.4151223720854,
98.7003817284338));
#29703=CARTESIAN_POINT('Ctrl Pts',(-11.6663040534074,-12.4078631071804,
98.6649661331026));
#29704=CARTESIAN_POINT('Ctrl Pts',(-11.719279568674,-12.4015749360366,98.6287647534647));
#29705=CARTESIAN_POINT('Ctrl Pts',(-11.8108343641753,-12.3907074207279,
98.5661998139274));
#29706=CARTESIAN_POINT('Ctrl Pts',(-11.9016543857439,-12.3828242789111,
98.5012454209961));
#29707=CARTESIAN_POINT('Ctrl Pts',(-11.991437135553,-12.3776871588067,98.4344604661188));
#29708=CARTESIAN_POINT('Ctrl Pts',(-12.0537689069902,-12.3741207076022,
98.3880949387573));
#29709=CARTESIAN_POINT('Ctrl Pts',(-12.1156007258684,-12.3718787930038,
98.3408460596308));
#29710=CARTESIAN_POINT('Ctrl Pts',(-12.1768266918443,-12.3708930987133,
98.29289321686));
#29711=CARTESIAN_POINT('Origin',(-2.55192432461455E-15,-20.8380434782609,
100.));
#29712=CARTESIAN_POINT('',(-2.57983136337902,-17.1656216833844,98.292893216895));
#29713=CARTESIAN_POINT('',(-2.57985201635105,-17.1655922755232,0.5));
#29714=CARTESIAN_POINT('',(-2.57985201635105,-17.1655922755232,100.));
#29715=CARTESIAN_POINT('',(2.57985201635104,-17.1655922755232,0.5));
#29716=CARTESIAN_POINT('Origin',(-2.55192432461455E-15,-20.8380434782609,
0.5));
#29717=CARTESIAN_POINT('',(2.57983420291488,-17.1656249920606,98.2928992166643));
#29718=CARTESIAN_POINT('',(2.57985201635104,-17.1655922755232,100.));
#29719=CARTESIAN_POINT('Ctrl Pts',(2.57983420291488,-17.1656249920606,98.2928992166643));
#29720=CARTESIAN_POINT('Ctrl Pts',(2.4892116886444,-17.1019995465655,98.3796187467301));
#29721=CARTESIAN_POINT('Ctrl Pts',(2.3946045185082,-17.0405846361733,98.4639979993635));
#29722=CARTESIAN_POINT('Ctrl Pts',(2.29603754132888,-16.9819052231602,98.5451592717554));
#29723=CARTESIAN_POINT('Ctrl Pts',(2.20329025421175,-16.9266904187466,98.6215285391179));
#29724=CARTESIAN_POINT('Ctrl Pts',(2.10703651916783,-16.8738971253428,98.6950495057112));
#29725=CARTESIAN_POINT('Ctrl Pts',(2.0072688812662,-16.8239841981541,98.7649644149723));
#29726=CARTESIAN_POINT('Ctrl Pts',(1.91489692774978,-16.7777712709252,98.8296965955089));
#29727=CARTESIAN_POINT('Ctrl Pts',(1.8195123779607,-16.7340272983991,98.891337936913));
#29728=CARTESIAN_POINT('Ctrl Pts',(1.72108984757851,-16.6931400079876,98.9492550268265));
#29729=CARTESIAN_POINT('Ctrl Pts',(1.66252076848856,-16.6688088824152,98.983720210831));
#29730=CARTESIAN_POINT('Ctrl Pts',(1.60287553638916,-16.6454898253045,99.0168659278811));
#29731=CARTESIAN_POINT('Ctrl Pts',(1.54214582819377,-16.6232694009981,99.048551829993));
#29732=CARTESIAN_POINT('Ctrl Pts',(1.50834082732673,-16.6109004717661,99.0661896876445));
#29733=CARTESIAN_POINT('Ctrl Pts',(1.47411579290756,-16.5988458341413,99.0834087225826));
#29734=CARTESIAN_POINT('Ctrl Pts',(1.43948739685436,-16.5871278596483,99.1001725241582));
#29735=CARTESIAN_POINT('Ctrl Pts',(1.33337731939881,-16.551221051283,99.151541010325));
#29736=CARTESIAN_POINT('Ctrl Pts',(1.22327810110348,-16.5184071918983,99.1987035934342));
#29737=CARTESIAN_POINT('Ctrl Pts',(1.10980264463643,-16.489434182122,99.240489893159));
#29738=CARTESIAN_POINT('Ctrl Pts',(1.00858832429893,-16.4635917349186,99.2777611415658));
#29739=CARTESIAN_POINT('Ctrl Pts',(0.904688737105505,-16.4408052848502,
99.3107542880671));
#29740=CARTESIAN_POINT('Ctrl Pts',(0.798561739816924,-16.4216158026087,
99.338614700467));
#29741=CARTESIAN_POINT('Ctrl Pts',(0.780189286660287,-16.4182937651197,
99.3434378287456));
#29742=CARTESIAN_POINT('Ctrl Pts',(0.761769227147023,-16.4150826446948,
99.3481021122734));
#29743=CARTESIAN_POINT('Ctrl Pts',(0.743304007781208,-16.4119834376879,
99.3526059457037));
#29744=CARTESIAN_POINT('Ctrl Pts',(0.642641649851918,-16.3950882425186,
99.3771584020724));
#29745=CARTESIAN_POINT('Ctrl Pts',(0.541062236488303,-16.3815877737481,
99.3968131856375));
#29746=CARTESIAN_POINT('Ctrl Pts',(0.438849030667434,-16.3715489101698,
99.4114442249363));
#29747=CARTESIAN_POINT('Ctrl Pts',(0.338466099151273,-16.3616898068673,
99.4258132744554));
#29748=CARTESIAN_POINT('Ctrl Pts',(0.23747133700468,-16.3551693456449,99.4353369845777));
#29749=CARTESIAN_POINT('Ctrl Pts',(0.13612476000251,-16.3520782871335,99.4398549403163));
#29750=CARTESIAN_POINT('Ctrl Pts',(0.0902193617685212,-16.3506781779624,
99.4419013691501));
#29751=CARTESIAN_POINT('Ctrl Pts',(0.0442417165457677,-16.3499820578742,
99.4429202057471));
#29752=CARTESIAN_POINT('Ctrl Pts',(-0.00178414082371589,-16.3500003546257,
99.4428936080771));
#29753=CARTESIAN_POINT('Ctrl Pts',(-0.00220644401206383,-16.3500005225047,
99.4428933640343));
#29754=CARTESIAN_POINT('Ctrl Pts',(-0.00262876716548478,-16.3500007510009,
99.4428930314822));
#29755=CARTESIAN_POINT('Ctrl Pts',(-0.00305111017540327,-16.3500010401123,
99.4428926104257));
#29756=CARTESIAN_POINT('Ctrl Pts',(-0.0947401221997488,-16.35006380507,
99.4428012007084));
#29757=CARTESIAN_POINT('Ctrl Pts',(-0.18732374215409,-16.3529858671848,
99.4385281272474));
#29758=CARTESIAN_POINT('Ctrl Pts',(-0.279483658282253,-16.3587250213924,
99.4301496922812));
#29759=CARTESIAN_POINT('Ctrl Pts',(-0.322405061827636,-16.3613979030974,
99.4262476250554));
#29760=CARTESIAN_POINT('Ctrl Pts',(-0.365234463339091,-16.3646813960556,
99.4214557128963));
#29761=CARTESIAN_POINT('Ctrl Pts',(-0.407839099049934,-16.3685690648589,
99.4157848279575));
#29762=CARTESIAN_POINT('Ctrl Pts',(-0.504270395105379,-16.3773684111056,
99.4029493518336));
#29763=CARTESIAN_POINT('Ctrl Pts',(-0.599122429574534,-16.3891631936093,
99.3857576708347));
#29764=CARTESIAN_POINT('Ctrl Pts',(-0.69237025112029,-16.4037252073042,
99.3645857641471));
#29765=CARTESIAN_POINT('Ctrl Pts',(-0.712154642550585,-16.4068148299267,
99.3600937204479));
#29766=CARTESIAN_POINT('Ctrl Pts',(-0.731866869233836,-16.4100289179416,
99.3554226501115));
#29767=CARTESIAN_POINT('Ctrl Pts',(-0.751506771534701,-16.4133651287016,
99.3505763727328));
#29768=CARTESIAN_POINT('Ctrl Pts',(-0.768810980041281,-16.4163045774693,
99.346306443435));
#29769=CARTESIAN_POINT('Ctrl Pts',(-0.786067148798637,-16.4193402078322,
99.3418984809088));
#29770=CARTESIAN_POINT('Ctrl Pts',(-0.803274493993886,-16.4224705426046,
99.3373550074189));
#29771=CARTESIAN_POINT('Ctrl Pts',(-0.885066655462472,-16.437350051573,
99.3157583861447));
#29772=CARTESIAN_POINT('Ctrl Pts',(-0.966042366928278,-16.4544870049868,
99.2909304823462));
#29773=CARTESIAN_POINT('Ctrl Pts',(-1.04570558262436,-16.473602141888,99.2633292101841));
#29774=CARTESIAN_POINT('Ctrl Pts',(-1.06594962075099,-16.4784596856972,
99.256315167365));
#29775=CARTESIAN_POINT('Ctrl Pts',(-1.0861090253284,-16.4834448422369,99.2491222220218));
#29776=CARTESIAN_POINT('Ctrl Pts',(-1.10617593665822,-16.4885527780128,
99.241758252988));
#29777=CARTESIAN_POINT('Ctrl Pts',(-1.21067589741909,-16.5151527404773,
99.2034098264448));
#29778=CARTESIAN_POINT('Ctrl Pts',(-1.31279762671789,-16.5451132691073,
99.1603383187126));
#29779=CARTESIAN_POINT('Ctrl Pts',(-1.41181620436576,-16.5778827216701,
99.1134130969983));
#29780=CARTESIAN_POINT('Ctrl Pts',(-1.42237752833916,-16.5813779123017,
99.1084080516743));
#29781=CARTESIAN_POINT('Ctrl Pts',(-1.4329035584962,-16.5849050809489,99.1033591233068));
#29782=CARTESIAN_POINT('Ctrl Pts',(-1.44339342091949,-16.5884635738797,
99.0982673376955));
#29783=CARTESIAN_POINT('Ctrl Pts',(-1.47741610194129,-16.6000051427791,
99.0817527075989));
#29784=CARTESIAN_POINT('Ctrl Pts',(-1.51105031263546,-16.6118734917002,
99.0647972731995));
#29785=CARTESIAN_POINT('Ctrl Pts',(-1.54426705507015,-16.6240461436618,
99.0474373027682));
#29786=CARTESIAN_POINT('Ctrl Pts',(-1.65397005242361,-16.6642480511353,
98.9901035412164));
#29787=CARTESIAN_POINT('Ctrl Pts',(-1.7594946302662,-16.7077102057232,98.9284409582433));
#29788=CARTESIAN_POINT('Ctrl Pts',(-1.86134539390795,-16.7541279961806,
98.8630104838176));
#29789=CARTESIAN_POINT('Ctrl Pts',(-1.92596432896475,-16.7835776348461,
98.821498300438));
#29790=CARTESIAN_POINT('Ctrl Pts',(-1.98910378648957,-16.8142174701363,
98.7784686515277));
#29791=CARTESIAN_POINT('Ctrl Pts',(-2.05088633004532,-16.8459741993693,
98.7340573318779));
#29792=CARTESIAN_POINT('Ctrl Pts',(-2.09899196596652,-16.8707008869837,
98.699477422232));
#29793=CARTESIAN_POINT('Ctrl Pts',(-2.14626276029159,-16.8960982022606,
98.6640680699512));
#29794=CARTESIAN_POINT('Ctrl Pts',(-2.19277810448147,-16.9221453115834,
98.6278739858466));
#29795=CARTESIAN_POINT('Ctrl Pts',(-2.2732023258176,-16.9671803107181,98.5652950437409));
#29796=CARTESIAN_POINT('Ctrl Pts',(-2.35127746875916,-17.0141953608637,
98.5003303240652));
#29797=CARTESIAN_POINT('Ctrl Pts',(-2.42689938963798,-17.0628202892722,
98.433538021466));
#29798=CARTESIAN_POINT('Ctrl Pts',(-2.4790592469673,-17.096359100492,98.3874683510083));
#29799=CARTESIAN_POINT('Ctrl Pts',(-2.53005139470365,-17.1306646048568,
98.3405281736901));
#29800=CARTESIAN_POINT('Ctrl Pts',(-2.57983136337902,-17.1656216833844,
98.292893216895));
#29801=CARTESIAN_POINT('Origin',(12.2482946431511,-16.8583313034371,100.));
#29802=CARTESIAN_POINT('',(12.1768414139071,-12.3708281240615,98.2929155812437));
#29803=CARTESIAN_POINT('',(8.00253786203375,-15.4036548382545,98.2928932187212));
#29804=CARTESIAN_POINT('Ctrl Pts',(12.1768223332082,-12.3708569612629,98.2928961772889));
#29805=CARTESIAN_POINT('Ctrl Pts',(11.9766556305925,-12.3740450279548,98.4496670611162));
#29806=CARTESIAN_POINT('Ctrl Pts',(11.7718386279247,-12.390541715911,98.5976778122645));
#29807=CARTESIAN_POINT('Ctrl Pts',(11.3497031910366,-12.455981009676,98.870667594539));
#29808=CARTESIAN_POINT('Ctrl Pts',(11.1323782772714,-12.5051975008586,98.9953666813422));
#29809=CARTESIAN_POINT('Ctrl Pts',(10.6948166070868,-12.6414901598492,99.2055148722619));
#29810=CARTESIAN_POINT('Ctrl Pts',(10.4709805367995,-12.7297564325018,99.2925877229868));
#29811=CARTESIAN_POINT('Ctrl Pts',(10.0271356237447,-12.9505917384117,99.4120512183375));
#29812=CARTESIAN_POINT('Ctrl Pts',(9.8121776999094,-13.0805177296113,99.4431642901975));
#29813=CARTESIAN_POINT('Ctrl Pts',(9.40304146226851,-13.3782342507087,99.4426185746832));
#29814=CARTESIAN_POINT('Ctrl Pts',(9.2084827250123,-13.5474714192234,99.4095817567495));
#29815=CARTESIAN_POINT('Ctrl Pts',(8.86697618306584,-13.8970925183944,99.2902945556315));
#29816=CARTESIAN_POINT('Ctrl Pts',(8.71497133569482,-14.081422575003,99.2037727159813));
#29817=CARTESIAN_POINT('Ctrl Pts',(8.44923508864959,-14.4577600834109,98.9917454068753));
#29818=CARTESIAN_POINT('Ctrl Pts',(8.33757587869828,-14.6461685366907,98.8686812585125));
#29819=CARTESIAN_POINT('Ctrl Pts',(8.1466428405253,-15.024254464469,98.5978506351621));
#29820=CARTESIAN_POINT('Ctrl Pts',(8.0672915044469,-15.2146587124184,98.4493425737989));
#29821=CARTESIAN_POINT('Ctrl Pts',(8.00253786221766,-15.4036548377177,98.2928932188135));
#29822=CARTESIAN_POINT('',(8.00253786221767,-15.4036548377177,0.5));
#29823=CARTESIAN_POINT('',(8.00253786221767,-15.4036548377177,100.));
#29824=CARTESIAN_POINT('',(12.1768261106186,-12.3708569011015,0.5));
#29825=CARTESIAN_POINT('Origin',(12.2482946431511,-16.8583313034371,0.5));
#29826=CARTESIAN_POINT('',(12.1768261106186,-12.3708569011015,100.));
#29827=CARTESIAN_POINT('Origin',(19.8181570368417,-6.43930956430665,100.));
#29828=CARTESIAN_POINT('',(15.5282646243346,-7.75803424826115,98.2928932168951));
#29829=CARTESIAN_POINT('',(15.5282302736771,-7.75804480287585,0.5));
#29830=CARTESIAN_POINT('',(15.5282302736771,-7.75804480287585,100.));
#29831=CARTESIAN_POINT('',(17.122666505727,-2.85087466042014,0.5));
#29832=CARTESIAN_POINT('Origin',(19.8181570368417,-6.43930956430665,0.5));
#29833=CARTESIAN_POINT('',(17.1226921163488,-2.8509017119705,98.2928992166648));
#29834=CARTESIAN_POINT('',(17.122666505727,-2.85087466042014,100.));
#29835=CARTESIAN_POINT('Ctrl Pts',(17.1226921163488,-2.8509017119705,98.2928992166648));
#29836=CARTESIAN_POINT('Ctrl Pts',(17.0341768248214,-2.91742750076124,98.3796187467353));
#29837=CARTESIAN_POINT('Ctrl Pts',(16.9465325507289,-2.98842601539211,98.4639979993731));
#29838=CARTESIAN_POINT('Ctrl Pts',(16.8602662415735,-3.06403584549337,98.5451592717689));
#29839=CARTESIAN_POINT('Ctrl Pts',(16.7790933541347,-3.13518144437395,98.621528539135));
#29840=CARTESIAN_POINT('Ctrl Pts',(16.6991399085219,-3.21041016145889,98.6950495057316));
#29841=CARTESIAN_POINT('Ctrl Pts',(16.6208399982677,-3.28987088086528,98.7649644149954));
#29842=CARTESIAN_POINT('Ctrl Pts',(16.5483443892456,-3.36344124931151,98.829696595535));
#29843=CARTESIAN_POINT('Ctrl Pts',(16.4772659522367,-3.44063971603582,98.8913379369416));
#29844=CARTESIAN_POINT('Ctrl Pts',(16.4079655937362,-3.52161023732113,98.9492550268571));
#29845=CARTESIAN_POINT('Ctrl Pts',(16.3667264774404,-3.56979401033572,98.9837202108507));
#29846=CARTESIAN_POINT('Ctrl Pts',(16.3261173458813,-3.61931401203589,99.0168659278907));
#29847=CARTESIAN_POINT('Ctrl Pts',(16.2862179546655,-3.67020490800025,99.0485518299934));
#29848=CARTESIAN_POINT('Ctrl Pts',(16.264008084157,-3.69853316502337,99.0661896876449));
#29849=CARTESIAN_POINT('Ctrl Pts',(16.2419673252237,-3.72735801914106,99.0834087225829));
#29850=CARTESIAN_POINT('Ctrl Pts',(16.220122106356,-3.75667052759827,99.1001725241585));
#29851=CARTESIAN_POINT('Ctrl Pts',(16.1531828850337,-3.84649139426061,99.1515410103551));
#29852=CARTESIAN_POINT('Ctrl Pts',(16.0879525206834,-3.94106193311628,99.1987035934887));
#29853=CARTESIAN_POINT('Ctrl Pts',(16.0253317064128,-4.04003035309249,99.2404898932312));
#29854=CARTESIAN_POINT('Ctrl Pts',(15.9694771335837,-4.12830513657678,99.2777611416079));
#29855=CARTESIAN_POINT('Ctrl Pts',(15.9156991936484,-4.22007811564716,99.3107542880842));
#29856=CARTESIAN_POINT('Ctrl Pts',(15.8646538658274,-4.31508101178553,99.3386147004664));
#29857=CARTESIAN_POINT('Ctrl Pts',(15.8558170201725,-4.33152768704044,99.343437828745));
#29858=CARTESIAN_POINT('Ctrl Pts',(15.8470709517407,-4.34805391388877,99.3481021122728));
#29859=CARTESIAN_POINT('Ctrl Pts',(15.8384173641326,-4.3646576734572,99.3526059457032));
#29860=CARTESIAN_POINT('Ctrl Pts',(15.7912426993732,-4.45517236249152,99.3771584020751));
#29861=CARTESIAN_POINT('Ctrl Pts',(15.7470132255631,-4.54760825122134,99.396813185642));
#29862=CARTESIAN_POINT('Ctrl Pts',(15.7058800812885,-4.64171660723027,99.4114442249414));
#29863=CARTESIAN_POINT('Ctrl Pts',(15.6654834850592,-4.73413981791697,99.4258132744614));
#29864=CARTESIAN_POINT('Ctrl Pts',(15.6280730600742,-4.82817661125299,99.4353369845832));
#29865=CARTESIAN_POINT('Ctrl Pts',(15.5938154741162,-4.92360774411853,99.4398549403198));
#29866=CARTESIAN_POINT('Ctrl Pts',(15.5782983429872,-4.96683371468982,99.4419013691512));
#29867=CARTESIAN_POINT('Ctrl Pts',(15.5634284197149,-5.0103459408207,99.442920205747));
#29868=CARTESIAN_POINT('Ctrl Pts',(15.54922304886,-5.05412478637214,99.4428936080771));
#29869=CARTESIAN_POINT('Ctrl Pts',(15.5490927096604,-5.05452647244875,99.4428933640342));
#29870=CARTESIAN_POINT('Ctrl Pts',(15.5489624219417,-5.05492819624499,99.4428930314822));
#29871=CARTESIAN_POINT('Ctrl Pts',(15.5488321857355,-5.05532995765703,99.4428926104257));
#29872=CARTESIAN_POINT('Ctrl Pts',(15.5205584158414,-5.14255078546346,99.4428012007084));
#29873=CARTESIAN_POINT('Ctrl Pts',(15.4947275500875,-5.23150600738526,99.4385281272465));
#29874=CARTESIAN_POINT('Ctrl Pts',(15.471706829809,-5.32092879235345,99.4301496922785));
#29875=CARTESIAN_POINT('Ctrl Pts',(15.4609854482567,-5.36257543874499,99.4262476250531));
#29876=CARTESIAN_POINT('Ctrl Pts',(15.4508732227073,-5.40432327525671,99.421455712895));
#29877=CARTESIAN_POINT('Ctrl Pts',(15.4414050589843,-5.44604404739281,99.4157848279575));
#29878=CARTESIAN_POINT('Ctrl Pts',(15.4199748252984,-5.54047480742042,99.4029493518322));
#29879=CARTESIAN_POINT('Ctrl Pts',(15.4018814394533,-5.63432924113464,99.3857576708312));
#29880=CARTESIAN_POINT('Ctrl Pts',(15.3869155759212,-5.72751309915976,99.3645857641404));
#29881=CARTESIAN_POINT('Ctrl Pts',(15.3837402684756,-5.7472839194373,99.3600937204433));
#29882=CARTESIAN_POINT('Ctrl Pts',(15.3807056347856,-5.76702456888336,99.3554226501091));
#29883=CARTESIAN_POINT('Ctrl Pts',(15.3778094961913,-5.78673417175797,99.3505763727328));
#29884=CARTESIAN_POINT('Ctrl Pts',(15.3752577835933,-5.80409979164077,99.346306443435));
#29885=CARTESIAN_POINT('Ctrl Pts',(15.3728123902272,-5.82144944475452,99.3418984809087));
#29886=CARTESIAN_POINT('Ctrl Pts',(15.3704721534172,-5.83878192917335,99.3373550074188));
#29887=CARTESIAN_POINT('Ctrl Pts',(15.3593482394826,-5.92116891844311,99.3157583861489));
#29888=CARTESIAN_POINT('Ctrl Pts',(15.350623579723,-6.00347700631512,99.2909304823557));
#29889=CARTESIAN_POINT('Ctrl Pts',(15.3441858677564,-6.08514812884863,99.2633292102));
#29890=CARTESIAN_POINT('Ctrl Pts',(15.342549914632,-6.10590241682891,99.2563151673759));
#29891=CARTESIAN_POINT('Ctrl Pts',(15.3410614816317,-6.1266156480231,99.2491222220274));
#29892=CARTESIAN_POINT('Ctrl Pts',(15.3397184006096,-6.1472788537819,99.2417582529879));
#29893=CARTESIAN_POINT('Ctrl Pts',(15.3327242044575,-6.25488406287628,99.2034098264416));
#29894=CARTESIAN_POINT('Ctrl Pts',(15.3296610105945,-6.36126591149707,99.1603383187055));
#29895=CARTESIAN_POINT('Ctrl Pts',(15.3302281887384,-6.46556449274991,99.1134130969867));
#29896=CARTESIAN_POINT('Ctrl Pts',(15.3302886839734,-6.47668898203059,99.1084080516665));
#29897=CARTESIAN_POINT('Ctrl Pts',(15.3303904984975,-6.48778978664755,99.1033591233028));
#29898=CARTESIAN_POINT('Ctrl Pts',(15.33053328063,-6.49886587344166,99.0982673376955));
#29899=CARTESIAN_POINT('Ctrl Pts',(15.3309963783101,-6.53478990686088,99.081752707599));
#29900=CARTESIAN_POINT('Ctrl Pts',(15.3318903061923,-6.57044546362382,99.0647972731996));
#29901=CARTESIAN_POINT('Ctrl Pts',(15.3332026482509,-6.60579801928925,99.0474373027683));
#29902=CARTESIAN_POINT('Ctrl Pts',(15.3375368438081,-6.72255484247992,98.9901035411749));
#29903=CARTESIAN_POINT('Ctrl Pts',(15.346262921273,-6.83634522432656,98.9284409581542));
#29904=CARTESIAN_POINT('Ctrl Pts',(15.3589352465191,-6.94755494294715,98.8630104836759));
#29905=CARTESIAN_POINT('Ctrl Pts',(15.3669751681779,-7.01811164095182,98.8214983003403));
#29906=CARTESIAN_POINT('Ctrl Pts',(15.3766042177888,-7.08762906319514,98.7784686514776));
#29907=CARTESIAN_POINT('Ctrl Pts',(15.3877148061349,-7.15620112277751,98.7340573318784));
#29908=CARTESIAN_POINT('Ctrl Pts',(15.3963658244922,-7.20959326797818,98.6994774222324));
#29909=CARTESIAN_POINT('Ctrl Pts',(15.4059126278986,-7.26239866698339,98.6640680699514));
#29910=CARTESIAN_POINT('Ctrl Pts',(15.4163108690968,-7.31468638761793,98.6278739858464));
#29911=CARTESIAN_POINT('Ctrl Pts',(15.4342892473289,-7.40509094744151,98.565295043754));
#29912=CARTESIAN_POINT('Ctrl Pts',(15.4548766711213,-7.49387327036325,98.500330324094));
#29913=CARTESIAN_POINT('Ctrl Pts',(15.4777532674335,-7.5808199201993,98.4335380215112));
#29914=CARTESIAN_POINT('Ctrl Pts',(15.4935322900585,-7.6407909550598,98.3874683510391));
#29915=CARTESIAN_POINT('Ctrl Pts',(15.5104013233044,-7.69988835331348,98.3405281737059));
#29916=CARTESIAN_POINT('Ctrl Pts',(15.5282646243346,-7.75803424826115,98.2928932168951));
#29917=CARTESIAN_POINT('Origin',(19.8181570368417,6.43930956430664,100.));
#29918=CARTESIAN_POINT('',(17.1226665061807,2.85087466007934,98.2928932187211));
#29919=CARTESIAN_POINT('',(17.122666505727,2.85087466042014,0.5));
#29920=CARTESIAN_POINT('',(17.122666505727,2.85087466042014,100.));
#29921=CARTESIAN_POINT('',(15.5282302736771,7.75804480287584,0.5));
#29922=CARTESIAN_POINT('Origin',(19.8181570368417,6.43930956430664,0.5));
#29923=CARTESIAN_POINT('',(15.528207634062,7.7580682497625,98.2929155812437));
#29924=CARTESIAN_POINT('',(15.5282302736771,7.75804480287584,100.));
#29925=CARTESIAN_POINT('Ctrl Pts',(15.5282291636101,7.75804119175414,98.2928961772889));
#29926=CARTESIAN_POINT('Ctrl Pts',(15.4694062823956,7.56668617809921,98.4496670611162));
#29927=CARTESIAN_POINT('Ctrl Pts',(15.4218036304123,7.36679587613452,98.5976778122644));
#29928=CARTESIAN_POINT('Ctrl Pts',(15.3535930732429,6.94509936424972,98.870667594539));
#29929=CARTESIAN_POINT('Ctrl Pts',(15.3332436462368,6.72320235668112,98.9953666813422));
#29930=CARTESIAN_POINT('Ctrl Pts',(15.3276516755189,6.26493973113448,99.2055148722619));
#29931=CARTESIAN_POINT('Ctrl Pts',(15.3424287396213,6.02478319962601,99.2925877229867));
#29932=CARTESIAN_POINT('Ctrl Pts',(15.4152999753342,5.5344197403566,99.4120512183375));
#29933=CARTESIAN_POINT('Ctrl Pts',(15.47244128436,5.28983326687212,99.4431642901975));
#29934=CARTESIAN_POINT('Ctrl Pts',(15.6291564713127,4.80872211748601,99.4426185746832));
#29935=CARTESIAN_POINT('Ctrl Pts',(15.7299886270117,4.5713886014654,99.4095817567495));
#29936=CARTESIAN_POINT('Ctrl Pts',(15.9569667264609,4.13855771815389,99.2902945556315));
#29937=CARTESIAN_POINT('Ctrl Pts',(16.0853029468825,3.93703139748707,99.2037727159813));
#29938=CARTESIAN_POINT('Ctrl Pts',(16.3611041702218,3.56800652240011,98.9917454068753));
#29939=CARTESIAN_POINT('Ctrl Pts',(16.5057866639851,3.40359088922421,98.8686812585125));
#29940=CARTESIAN_POINT('Ctrl Pts',(16.8063661957351,3.10516780207624,98.5978506351621));
#29941=CARTESIAN_POINT('Ctrl Pts',(16.9629304851031,2.97086204840461,98.4493425737988));
#29942=CARTESIAN_POINT('Ctrl Pts',(17.122666505727,2.85087466042014,98.2928932188135));
#29943=CARTESIAN_POINT('Origin',(12.2482946431511,16.8583313034371,100.));
#29944=CARTESIAN_POINT('',(12.1768261122223,12.3708569010759,98.2928932196637));
#29945=CARTESIAN_POINT('',(12.1768261106186,12.3708569011015,0.5));
#29946=CARTESIAN_POINT('',(12.1768261106186,12.3708569011015,100.));
#29947=CARTESIAN_POINT('',(8.00253786221767,15.4036548377177,0.5));
#29948=CARTESIAN_POINT('Origin',(12.2482946431511,16.8583313034371,0.5));
#29949=CARTESIAN_POINT('',(8.00250696667699,15.4036606035888,98.2929148412894));
#29950=CARTESIAN_POINT('',(8.00253786221767,15.4036548377177,100.));
#29951=CARTESIAN_POINT('Ctrl Pts',(8.00250708598551,15.4036602554268,98.2929146461936));
#29952=CARTESIAN_POINT('Ctrl Pts',(8.04095434018177,15.291393927702,98.3858632379257));
#29953=CARTESIAN_POINT('Ctrl Pts',(8.08445379523924,15.1789643815694,98.4757075594465));
#29954=CARTESIAN_POINT('Ctrl Pts',(8.13349045375344,15.0664065104534,98.5618687047919));
#29955=CARTESIAN_POINT('Ctrl Pts',(8.14594002061313,15.0378299967899,98.583743542356));
#29956=CARTESIAN_POINT('Ctrl Pts',(8.15874627805921,15.0092451974279,98.6053811116386));
#29957=CARTESIAN_POINT('Ctrl Pts',(8.17191669602578,14.9806526573416,98.6267722404462));
#29958=CARTESIAN_POINT('Ctrl Pts',(8.19442659046237,14.9317844239531,98.6633323596894));
#29959=CARTESIAN_POINT('Ctrl Pts',(8.21808777573002,14.8827759730826,98.6992365502331));
#29960=CARTESIAN_POINT('Ctrl Pts',(8.24287820376329,14.8337655789499,98.7343285177238));
#29961=CARTESIAN_POINT('Ctrl Pts',(8.29540418081832,14.7299223200028,98.8086814041185));
#29962=CARTESIAN_POINT('Ctrl Pts',(8.35322906335348,14.6256182642871,98.8796681588396));
#29963=CARTESIAN_POINT('Ctrl Pts',(8.41624979623094,14.5221819933805,98.9457243517224));
#29964=CARTESIAN_POINT('Ctrl Pts',(8.45042299051297,14.4660933441359,98.981543533916));
#29965=CARTESIAN_POINT('Ctrl Pts',(8.48612332306307,14.4102605388777,99.0159124054391));
#29966=CARTESIAN_POINT('Ctrl Pts',(8.52333003766506,14.3548990672716,99.0485791162114));
#29967=CARTESIAN_POINT('Ctrl Pts',(8.54347127793547,14.3249300492255,99.0662627004124));
#29968=CARTESIAN_POINT('Ctrl Pts',(8.56405612172782,14.2950703500545,99.0834771132441));
#29969=CARTESIAN_POINT('Ctrl Pts',(8.58510094647066,14.2653257640177,99.100197897678));
#29970=CARTESIAN_POINT('Ctrl Pts',(8.64085775874532,14.1865195339774,99.1444984632641));
#29971=CARTESIAN_POINT('Ctrl Pts',(8.69986277604658,14.1084893186493,99.1853565450778));
#29972=CARTESIAN_POINT('Ctrl Pts',(8.76251977964181,14.0312399826539,99.2223453246317));
#29973=CARTESIAN_POINT('Ctrl Pts',(8.82234975489255,13.9574760680786,99.257665203309));
#29974=CARTESIAN_POINT('Ctrl Pts',(8.88550949800824,13.8844241448105,99.289457225426));
#29975=CARTESIAN_POINT('Ctrl Pts',(8.95238110252481,13.8120961796908,99.3173134272115));
#29976=CARTESIAN_POINT('Ctrl Pts',(8.96841979763654,13.7947488139592,99.3239945459111));
#29977=CARTESIAN_POINT('Ctrl Pts',(8.98467216422562,13.77744313058,99.3304490804175));
#29978=CARTESIAN_POINT('Ctrl Pts',(9.00114376230894,13.7601793662716,99.3366710553152));
#29979=CARTESIAN_POINT('Ctrl Pts',(9.01384496169295,13.7468673299112,99.3414688013104));
#29980=CARTESIAN_POINT('Ctrl Pts',(9.0266780465601,13.733584418606,99.3461220848251));
#29981=CARTESIAN_POINT('Ctrl Pts',(9.03963548955907,13.7203394312888,99.3506266622461));
#29982=CARTESIAN_POINT('Ctrl Pts',(9.11972744908153,13.6384701158563,99.3784701520841));
#29983=CARTESIAN_POINT('Ctrl Pts',(9.2042699094525,13.5583572449624,99.4004995600338));
#29984=CARTESIAN_POINT('Ctrl Pts',(9.29128918150769,13.4821421839037,99.4158205242226));
#29985=CARTESIAN_POINT('Ctrl Pts',(9.39222822782232,13.39373561147,99.4335922600383));
#29986=CARTESIAN_POINT('Ctrl Pts',(9.49729440462541,13.3096962059213,99.4426890000595));
#29987=CARTESIAN_POINT('Ctrl Pts',(9.60659271286559,13.2301161534923,99.4428904203957));
#29988=CARTESIAN_POINT('Ctrl Pts',(9.60682851186603,13.2299444683389,99.4428908549378));
#29989=CARTESIAN_POINT('Ctrl Pts',(9.60706433486258,13.2297728014511,99.4428912473282));
#29990=CARTESIAN_POINT('Ctrl Pts',(9.60730018182523,13.2296011528498,99.4428915975688));
#29991=CARTESIAN_POINT('Ctrl Pts',(9.68141111896967,13.1756634698734,99.443001654775));
#29992=CARTESIAN_POINT('Ctrl Pts',(9.75791369194048,13.1235161930199,99.4389375211787));
#29993=CARTESIAN_POINT('Ctrl Pts',(9.83576642335548,13.0738739726876,99.4307630339869));
#29994=CARTESIAN_POINT('Ctrl Pts',(9.87237363862743,13.0505316517021,99.4269192997091));
#29995=CARTESIAN_POINT('Ctrl Pts',(9.90927903494219,13.027742911758,99.4221673968387));
#29996=CARTESIAN_POINT('Ctrl Pts',(9.94637331208392,13.005580020478,99.4165172327955));
#29997=CARTESIAN_POINT('Ctrl Pts',(10.0295053402483,12.9559107387434,99.4038546435077));
#29998=CARTESIAN_POINT('Ctrl Pts',(10.1131220126551,12.9095945146256,99.3868321498127));
#29999=CARTESIAN_POINT('Ctrl Pts',(10.1970690548928,12.8664609300696,99.3658258363096));
#30000=CARTESIAN_POINT('Ctrl Pts',(10.2150684963252,12.8572124752308,99.3613217835219));
#30001=CARTESIAN_POINT('Ctrl Pts',(10.2330831050249,12.848110220653,99.356634731462));
#30002=CARTESIAN_POINT('Ctrl Pts',(10.2511113268446,12.8391523023418,99.3517686237608));
#30003=CARTESIAN_POINT('Ctrl Pts',(10.2669187778883,12.8312978474447,99.347501937893));
#30004=CARTESIAN_POINT('Ctrl Pts',(10.282743992679,12.8235507352674,99.3430956262505));
#30005=CARTESIAN_POINT('Ctrl Pts',(10.2985854655186,12.8159101990171,99.338552249982));
#30006=CARTESIAN_POINT('Ctrl Pts',(10.3738460618529,12.7796110922143,99.3169673120915));
#30007=CARTESIAN_POINT('Ctrl Pts',(10.4497789726769,12.7456422248509,99.2921178033808));
#30008=CARTESIAN_POINT('Ctrl Pts',(10.5258154870433,12.7140687420573,99.2644650244466));
#30009=CARTESIAN_POINT('Ctrl Pts',(10.5448521424921,12.7061639410775,99.257541818811));
#30010=CARTESIAN_POINT('Ctrl Pts',(10.5638953135331,12.6984091102545,99.250443088872));
#30011=CARTESIAN_POINT('Ctrl Pts',(10.5829361512678,12.6908049207666,99.2431764205676));
#30012=CARTESIAN_POINT('Ctrl Pts',(10.6820892558461,12.6512069258659,99.2053360307508));
#30013=CARTESIAN_POINT('Ctrl Pts',(10.7813009537869,12.6156428243816,99.162858290905));
#30014=CARTESIAN_POINT('Ctrl Pts',(10.8797010335179,12.5840907769962,99.1165798460081));
#30015=CARTESIAN_POINT('Ctrl Pts',(10.8915595472027,12.580288337133,99.1110026800788));
#30016=CARTESIAN_POINT('Ctrl Pts',(10.9034062979255,12.5765441851188,99.1053702615652));
#30017=CARTESIAN_POINT('Ctrl Pts',(10.9152397813687,12.5728582981514,99.0996840124348));
#30018=CARTESIAN_POINT('Ctrl Pts',(10.9496077250952,12.5621533897882,99.0831694593815));
#30019=CARTESIAN_POINT('Ctrl Pts',(10.9838534531501,12.5519431297429,99.0662118234553));
#30020=CARTESIAN_POINT('Ctrl Pts',(11.0179405472128,12.5422262222296,99.0488473569641));
#30021=CARTESIAN_POINT('Ctrl Pts',(11.1286979038281,12.510653598624,98.9924259323609));
#30022=CARTESIAN_POINT('Ctrl Pts',(11.2380248633315,12.4840338074687,98.9317993629735));
#30023=CARTESIAN_POINT('Ctrl Pts',(11.3461476367307,12.4618433879634,98.867503097581));
#30024=CARTESIAN_POINT('Ctrl Pts',(11.4178105089765,12.4471357630283,98.82488806924));
#30025=CARTESIAN_POINT('Ctrl Pts',(11.4889441178525,12.4343747574872,98.78066013646));
#30026=CARTESIAN_POINT('Ctrl Pts',(11.559611526168,12.4234165163235,98.7349665698168));
#30027=CARTESIAN_POINT('Ctrl Pts',(11.6130987298846,12.4151223720855,98.7003817284332));
#30028=CARTESIAN_POINT('Ctrl Pts',(11.6663040534072,12.4078631071804,98.6649661331023));
#30029=CARTESIAN_POINT('Ctrl Pts',(11.719279568674,12.4015749360366,98.6287647534646));
#30030=CARTESIAN_POINT('Ctrl Pts',(11.8108343641639,12.3907074207293,98.5661998139358));
#30031=CARTESIAN_POINT('Ctrl Pts',(11.9016543857213,12.3828242789131,98.5012454210128));
#30032=CARTESIAN_POINT('Ctrl Pts',(11.9914371355195,12.3776871588086,98.434460466144));
#30033=CARTESIAN_POINT('Ctrl Pts',(12.053768906968,12.3741207076031,98.3880949387745));
#30034=CARTESIAN_POINT('Ctrl Pts',(12.1156007258574,12.371878793004,98.3408460596394));
#30035=CARTESIAN_POINT('Ctrl Pts',(12.1768266918443,12.3708930987134,98.2928932168601));
#30036=CARTESIAN_POINT('Origin',(0.,20.8380434782609,100.));
#30037=CARTESIAN_POINT('',(2.57983136337907,17.1656216833844,98.292893216895));
#30038=CARTESIAN_POINT('',(2.57985201635105,17.1655922755232,0.5));
#30039=CARTESIAN_POINT('',(2.57985201635105,17.1655922755232,100.));
#30040=CARTESIAN_POINT('',(-2.57985201635105,17.1655922755232,0.5));
#30041=CARTESIAN_POINT('Origin',(0.,20.8380434782609,0.5));
#30042=CARTESIAN_POINT('',(-2.57983420291524,17.1656249920608,98.292899216665));
#30043=CARTESIAN_POINT('',(-2.57985201635105,17.1655922755232,100.));
#30044=CARTESIAN_POINT('Ctrl Pts',(-2.57983420291524,17.1656249920608,98.292899216665));
#30045=CARTESIAN_POINT('Ctrl Pts',(-2.48921168864423,17.1019995465654,98.3796187467316));
#30046=CARTESIAN_POINT('Ctrl Pts',(-2.39460451850736,17.0405846361727,98.4639979993656));
#30047=CARTESIAN_POINT('Ctrl Pts',(-2.29603754132725,16.9819052231592,98.5451592717579));
#30048=CARTESIAN_POINT('Ctrl Pts',(-2.20329025420896,16.9266904187451,98.6215285391212));
#30049=CARTESIAN_POINT('Ctrl Pts',(-2.10703651916376,16.8738971253407,98.6950495057151));
#30050=CARTESIAN_POINT('Ctrl Pts',(-2.00726888126077,16.8239841981514,98.7649644149767));
#30051=CARTESIAN_POINT('Ctrl Pts',(-1.91489692774296,16.7777712709219,98.829696595514));
#30052=CARTESIAN_POINT('Ctrl Pts',(-1.81951237795242,16.7340272983954,98.8913379369186));
#30053=CARTESIAN_POINT('Ctrl Pts',(-1.72108984756871,16.6931400079835,98.9492550268325));
#30054=CARTESIAN_POINT('Ctrl Pts',(-1.6625207684819,16.6688088824126,98.9837202108348));
#30055=CARTESIAN_POINT('Ctrl Pts',(-1.60287553638577,16.6454898253033,99.0168659278829));
#30056=CARTESIAN_POINT('Ctrl Pts',(-1.54214582819379,16.6232694009981,99.048551829993));
#30057=CARTESIAN_POINT('Ctrl Pts',(-1.50834082732675,16.6109004717661,99.0661896876445));
#30058=CARTESIAN_POINT('Ctrl Pts',(-1.47411579290757,16.5988458341413,99.0834087225826));
#30059=CARTESIAN_POINT('Ctrl Pts',(-1.43948739685437,16.5871278596483,99.1001725241582));
#30060=CARTESIAN_POINT('Ctrl Pts',(-1.33337731940238,16.5512210512842,99.1515410103233));
#30061=CARTESIAN_POINT('Ctrl Pts',(-1.22327810111083,16.5184071919005,99.198703593431));
#30062=CARTESIAN_POINT('Ctrl Pts',(-1.10980264464779,16.4894341821249,99.2404898931548));
#30063=CARTESIAN_POINT('Ctrl Pts',(-1.00858832430666,16.4635917349203,99.2777611415633));
#30064=CARTESIAN_POINT('Ctrl Pts',(-0.904688737109412,16.4408052848509,
99.310754288066));
#30065=CARTESIAN_POINT('Ctrl Pts',(-0.798561739816899,16.4216158026087,
99.3386147004669));
#30066=CARTESIAN_POINT('Ctrl Pts',(-0.780189286660266,16.4182937651197,
99.3434378287455));
#30067=CARTESIAN_POINT('Ctrl Pts',(-0.761769227147002,16.4150826446948,
99.3481021122732));
#30068=CARTESIAN_POINT('Ctrl Pts',(-0.743304007781183,16.4119834376879,
99.3526059457036));
#30069=CARTESIAN_POINT('Ctrl Pts',(-0.64264164986231,16.3950882425204,99.3771584020698));
#30070=CARTESIAN_POINT('Ctrl Pts',(-0.541062236509303,16.3815877737509,
99.3968131856337));
#30071=CARTESIAN_POINT('Ctrl Pts',(-0.438849030699141,16.371548910173,99.4114442249324));
#30072=CARTESIAN_POINT('Ctrl Pts',(-0.33846609919671,16.361689806871,99.4258132744509));
#30073=CARTESIAN_POINT('Ctrl Pts',(-0.237471337063981,16.3551693456484,
99.4353369845739));
#30074=CARTESIAN_POINT('Ctrl Pts',(-0.136124760075694,16.3520782871358,
99.4398549403142));
#30075=CARTESIAN_POINT('Ctrl Pts',(-0.0902193618173922,16.3506781779631,
99.4419013691502));
#30076=CARTESIAN_POINT('Ctrl Pts',(-0.0442417165702345,16.3499820578742,
99.4429202057482));
#30077=CARTESIAN_POINT('Ctrl Pts',(0.0017841408237108,16.3500003546257,
99.4428936080781));
#30078=CARTESIAN_POINT('Ctrl Pts',(0.00220644401206086,16.3500005225047,
99.4428933640352));
#30079=CARTESIAN_POINT('Ctrl Pts',(0.00262876716548417,16.3500007510009,
99.4428930314832));
#30080=CARTESIAN_POINT('Ctrl Pts',(0.00305111017540478,16.3500010401123,
99.4428926104267));
#30081=CARTESIAN_POINT('Ctrl Pts',(0.0947401221956442,16.35006380507,99.442801200709));
#30082=CARTESIAN_POINT('Ctrl Pts',(0.187323742145935,16.3529858671845,99.4385281272487));
#30083=CARTESIAN_POINT('Ctrl Pts',(0.279483658270004,16.3587250213916,99.4301496922833));
#30084=CARTESIAN_POINT('Ctrl Pts',(0.322405061819553,16.3613979030968,99.4262476250572));
#30085=CARTESIAN_POINT('Ctrl Pts',(0.365234463335138,16.3646813960552,99.4214557128977));
#30086=CARTESIAN_POINT('Ctrl Pts',(0.407839099050017,16.3685690648589,99.4157848279582));
#30087=CARTESIAN_POINT('Ctrl Pts',(0.504270395098256,16.3773684111049,99.402949351835));
#30088=CARTESIAN_POINT('Ctrl Pts',(0.599122429560623,16.3891631936075,99.3857576708374));
#30089=CARTESIAN_POINT('Ctrl Pts',(0.692370251099814,16.403725207301,99.3645857641517));
#30090=CARTESIAN_POINT('Ctrl Pts',(0.712154642536984,16.4068148299245,99.3600937204511));
#30091=CARTESIAN_POINT('Ctrl Pts',(0.731866869227064,16.4100289179404,99.3554226501132));
#30092=CARTESIAN_POINT('Ctrl Pts',(0.751506771534702,16.4133651287016,99.3505763727328));
#30093=CARTESIAN_POINT('Ctrl Pts',(0.768810980041277,16.4163045774693,99.346306443435));
#30094=CARTESIAN_POINT('Ctrl Pts',(0.786067148798632,16.4193402078322,99.3418984809087));
#30095=CARTESIAN_POINT('Ctrl Pts',(0.803274493993878,16.4224705426046,99.3373550074188));
#30096=CARTESIAN_POINT('Ctrl Pts',(0.885066655452863,16.4373500515712,99.3157583861473));
#30097=CARTESIAN_POINT('Ctrl Pts',(0.96604236690926,16.4544870049828,99.290930482352));
#30098=CARTESIAN_POINT('Ctrl Pts',(1.0457055825963,16.4736021418813,99.2633292101938));
#30099=CARTESIAN_POINT('Ctrl Pts',(1.06594962073236,16.4784596856926,99.2563151673717));
#30100=CARTESIAN_POINT('Ctrl Pts',(1.08610902531913,16.4834448422345,99.2491222220252));
#30101=CARTESIAN_POINT('Ctrl Pts',(1.10617593665823,16.4885527780128,99.241758252988));
#30102=CARTESIAN_POINT('Ctrl Pts',(1.21067589744461,16.5151527404838,99.2034098264354));
#30103=CARTESIAN_POINT('Ctrl Pts',(1.31279762676775,16.5451132691219,99.1603383186916));
#30104=CARTESIAN_POINT('Ctrl Pts',(1.41181620443827,16.5778827216941,99.113413096964));
#30105=CARTESIAN_POINT('Ctrl Pts',(1.42237752838734,16.5813779123178,99.1084080516512));
#30106=CARTESIAN_POINT('Ctrl Pts',(1.43290355852021,16.584905080957,99.1033591232951));
#30107=CARTESIAN_POINT('Ctrl Pts',(1.4433934209195,16.5884635738797,99.0982673376954));
#30108=CARTESIAN_POINT('Ctrl Pts',(1.47741610194125,16.6000051427791,99.0817527075989));
#30109=CARTESIAN_POINT('Ctrl Pts',(1.51105031263543,16.6118734917002,99.0647972731996));
#30110=CARTESIAN_POINT('Ctrl Pts',(1.54426705507019,16.6240461436619,99.0474373027683));
#30111=CARTESIAN_POINT('Ctrl Pts',(1.65397005247796,16.6642480511552,98.9901035411882));
#30112=CARTESIAN_POINT('Ctrl Pts',(1.75949463037048,16.7077102057661,98.928440958183));
#30113=CARTESIAN_POINT('Ctrl Pts',(1.86134539405867,16.7541279962493,98.8630104837217));
#30114=CARTESIAN_POINT('Ctrl Pts',(1.92596432906305,16.7835776348937,98.821498300372));
#30115=CARTESIAN_POINT('Ctrl Pts',(1.98910378653781,16.814217470161,98.778468651494));
#30116=CARTESIAN_POINT('Ctrl Pts',(2.05088633004559,16.8459741993694,98.7340573318784));
#30117=CARTESIAN_POINT('Ctrl Pts',(2.09899196596664,16.8707008869838,98.6994774222324));
#30118=CARTESIAN_POINT('Ctrl Pts',(2.14626276029161,16.8960982022606,98.6640680699515));
#30119=CARTESIAN_POINT('Ctrl Pts',(2.19277810448148,16.9221453115834,98.6278739858466));
#30120=CARTESIAN_POINT('Ctrl Pts',(2.2732023258085,16.967180310713,98.5652950437475));
#30121=CARTESIAN_POINT('Ctrl Pts',(2.35127746874125,17.0141953608528,98.5003303240798));
#30122=CARTESIAN_POINT('Ctrl Pts',(2.42689938961185,17.0628202892553,98.4335380214889));
#30123=CARTESIAN_POINT('Ctrl Pts',(2.47905924695026,17.0963591004805,98.3874683510239));
#30124=CARTESIAN_POINT('Ctrl Pts',(2.53005139469532,17.1306646048509,98.3405281736981));
#30125=CARTESIAN_POINT('Ctrl Pts',(2.57983136337907,17.1656216833844,98.292893216895));
#30126=CARTESIAN_POINT('Ctrl Pts',(7.61153061250581,15.7863147967496,98.4745004885114));
#30127=CARTESIAN_POINT('Ctrl Pts',(7.88836095469125,15.7787835827682,98.3610536502059));
#30128=CARTESIAN_POINT('Ctrl Pts',(7.9381581147024,15.6072288420487,98.1209470979181));
#30129=CARTESIAN_POINT('Ctrl Pts',(7.68185024283006,15.5529265513645,98.6541872523935));
#30130=CARTESIAN_POINT('Ctrl Pts',(7.94367437493435,15.5575146677548,98.5339912542893));
#30131=CARTESIAN_POINT('Ctrl Pts',(7.99873405832662,15.3985404288948,98.3006281519141));
#30132=CARTESIAN_POINT('Ctrl Pts',(7.77058558273983,15.3193429185922,98.8238114502906));
#30133=CARTESIAN_POINT('Ctrl Pts',(8.01739572281313,15.3332616605645,98.6995854322395));
#30134=CARTESIAN_POINT('Ctrl Pts',(8.07554514465371,15.1898709314151,98.4702580602194));
#30135=CARTESIAN_POINT('Ctrl Pts',(7.99242980712988,14.8502894771665,99.1368088098188));
#30136=CARTESIAN_POINT('Ctrl Pts',(8.20881182371915,14.8837031652933,99.0046294469941));
#30137=CARTESIAN_POINT('Ctrl Pts',(8.26829617652396,14.7714171710724,98.7832554187034));
#30138=CARTESIAN_POINT('Ctrl Pts',(8.12737169382821,14.6123994681448,99.2813501417123));
#30139=CARTESIAN_POINT('Ctrl Pts',(8.327762510152,14.6553398972786,99.1461712456963));
#30140=CARTESIAN_POINT('Ctrl Pts',(8.38583875689921,14.5594769234819,98.9277967516668));
#30141=CARTESIAN_POINT('Ctrl Pts',(8.44228186665902,14.1522925726334,99.5228530262281));
#30142=CARTESIAN_POINT('Ctrl Pts',(8.61067658867425,14.2156092191238,99.3819067332058));
#30143=CARTESIAN_POINT('Ctrl Pts',(8.66083652547866,14.1502985880832,99.1692996350871));
#30144=CARTESIAN_POINT('Ctrl Pts',(8.622381227697,13.9285751457638,99.6211970158389));
#30145=CARTESIAN_POINT('Ctrl Pts',(8.77477430608659,14.0016497079293,99.4784987699955));
#30146=CARTESIAN_POINT('Ctrl Pts',(8.81839581871033,13.9517156783975,99.2676436259638));
#30147=CARTESIAN_POINT('Ctrl Pts',(8.93504150578053,13.6041086188711,99.7247006505005));
#30148=CARTESIAN_POINT('Ctrl Pts',(9.062909374557,13.6933479875451,99.5798189693937));
#30149=CARTESIAN_POINT('Ctrl Pts',(9.09252380741147,13.6644048462732,99.3711472595481));
#30150=CARTESIAN_POINT('Ctrl Pts',(9.04643201266469,13.4980463524892,99.7515464581428));
#30151=CARTESIAN_POINT('Ctrl Pts',(9.16590083805353,13.5929484631972,99.6061008493641));
#30152=CARTESIAN_POINT('Ctrl Pts',(9.19027681092598,13.5706128359882,99.397993067634));
#30153=CARTESIAN_POINT('Ctrl Pts',(9.27641719553063,13.2976623200444,99.7871410858034));
#30154=CARTESIAN_POINT('Ctrl Pts',(9.37920676320414,13.4041562061325,99.6408876188391));
#30155=CARTESIAN_POINT('Ctrl Pts',(9.39230696146117,13.3936667965264,99.4335876951257));
#30156=CARTESIAN_POINT('Ctrl Pts',(9.3959224352673,13.2023470673548,99.7962421951754));
#30157=CARTESIAN_POINT('Ctrl Pts',(9.49053581390408,13.314627456823,99.6498002056397));
#30158=CARTESIAN_POINT('Ctrl Pts',(9.4973820058399,13.3096324234838,99.4426888046372));
#30159=CARTESIAN_POINT('Ctrl Pts',(9.64409776558328,13.0216618073134,99.7966442229662));
#30160=CARTESIAN_POINT('Ctrl Pts',(9.72219875439392,13.1459331194971,99.6501931431456));
#30161=CARTESIAN_POINT('Ctrl Pts',(9.71580342119465,13.1505998825527,99.4430908323178));
#30162=CARTESIAN_POINT('Ctrl Pts',(9.77381197449083,12.9356824620425,99.7877849805069));
#30163=CARTESIAN_POINT('Ctrl Pts',(9.84373626500592,13.066044592077,99.6415170968012));
#30164=CARTESIAN_POINT('Ctrl Pts',(9.83007072703063,13.0750678730396,99.4342315896588));
#30165=CARTESIAN_POINT('Ctrl Pts',(10.0376062905058,12.7771593103382,99.7523547967176));
#30166=CARTESIAN_POINT('Ctrl Pts',(10.0912047848047,12.9199070101992,99.606890957529));
#30167=CARTESIAN_POINT('Ctrl Pts',(10.0626757487172,12.9360922565949,99.3988014063792));
#30168=CARTESIAN_POINT('Ctrl Pts',(10.1706575690794,12.7050827268414,99.7260859669308));
#30169=CARTESIAN_POINT('Ctrl Pts',(10.2163999615547,12.8539677361419,99.581174605592));
#30170=CARTESIAN_POINT('Ctrl Pts',(10.1801044201997,12.8730550738083,99.3725325760877));
#30171=CARTESIAN_POINT('Ctrl Pts',(10.5730247519988,12.5085765171446,99.6241384720945));
#30172=CARTESIAN_POINT('Ctrl Pts',(10.5959433339676,12.6756716426711,99.4813799591424));
#30173=CARTESIAN_POINT('Ctrl Pts',(10.5355461919893,12.7016211074059,99.2705850820007));
#30174=CARTESIAN_POINT('Ctrl Pts',(10.8489658974355,12.4029669023367,99.5236562902281));
#30175=CARTESIAN_POINT('Ctrl Pts',(10.8572640774196,12.5825975767439,99.3826839740385));
#30176=CARTESIAN_POINT('Ctrl Pts',(10.7797437745,12.610127671606,99.1701028989522));
#30177=CARTESIAN_POINT('Ctrl Pts',(11.386390404632,12.2448379356151,99.281082704477));
#30178=CARTESIAN_POINT('Ctrl Pts',(11.3652836467711,12.4487162064099,99.1459030339923));
#30179=CARTESIAN_POINT('Ctrl Pts',(11.256110836745,12.4743323246936,98.9275293145664));
#30180=CARTESIAN_POINT('Ctrl Pts',(11.6491602608155,12.1909944678527,99.1393951997099));
#30181=CARTESIAN_POINT('Ctrl Pts',(11.6143348897634,12.4069069268349,99.0071411174895));
#30182=CARTESIAN_POINT('Ctrl Pts',(11.489403766598,12.4288617015343,98.7858418086567));
#30183=CARTESIAN_POINT('Ctrl Pts',(12.1662817650119,12.1242950353392,98.825202900069));
#30184=CARTESIAN_POINT('Ctrl Pts',(12.1033811314414,12.3632333592681,98.7009299069312));
#30185=CARTESIAN_POINT('Ctrl Pts',(11.9491322142495,12.3742909202748,98.4716495099356));
#30186=CARTESIAN_POINT('Ctrl Pts',(12.4202878510312,12.1120529425571,98.6524117207793));
#30187=CARTESIAN_POINT('Ctrl Pts',(12.3435537205772,12.3625816382562,98.5323055644749));
#30188=CARTESIAN_POINT('Ctrl Pts',(12.1752607824306,12.3657340555541,98.2988642625951));
#30189=CARTESIAN_POINT('Ctrl Pts',(12.6613982812294,12.1172313198433,98.4746383405503));
#30190=CARTESIAN_POINT('Ctrl Pts',(12.5687009849841,12.378177146358,98.3611876972422));
#30191=CARTESIAN_POINT('Ctrl Pts',(12.3901642949232,12.3725306764959,98.121084949957));
#30192=CARTESIAN_POINT('Ctrl Pts',(12.1768261122223,12.3708569010759,98.2928932196637));
#30193=CARTESIAN_POINT('Ctrl Pts',(12.2099878174149,12.3703287601505,98.3104738976694));
#30194=CARTESIAN_POINT('Ctrl Pts',(12.2429433132094,12.366507919976,98.327944020444));
#30195=CARTESIAN_POINT('Ctrl Pts',(12.2752735670645,12.3594661072471,98.3450378051381));
#30196=CARTESIAN_POINT('Ctrl Pts',(12.3046862235392,12.3530597728063,98.360588985754));
#30197=CARTESIAN_POINT('Ctrl Pts',(12.3335840639558,12.3439862285568,98.3758286876098));
#30198=CARTESIAN_POINT('Ctrl Pts',(12.3616325402612,12.3322664746469,98.3905567852375));
#30199=CARTESIAN_POINT('Ctrl Pts',(12.3872721168772,12.3215532535428,98.404019983146));
#30200=CARTESIAN_POINT('Ctrl Pts',(12.4122030444781,12.3086274763191,98.4170556799153));
#30201=CARTESIAN_POINT('Ctrl Pts',(12.4361292621088,12.2934948895151,98.429511010888));
#30202=CARTESIAN_POINT('Ctrl Pts',(12.4577825179125,12.2797998802121,98.4407831004357));
#30203=CARTESIAN_POINT('Ctrl Pts',(12.4786130500859,12.2642963979525,98.4515798546202));
#30204=CARTESIAN_POINT('Ctrl Pts',(12.4983593286873,12.2469958685832,98.4617879670104));
#30205=CARTESIAN_POINT('Ctrl Pts',(12.5081070139959,12.2384555193169,98.4668271680256));
#30206=CARTESIAN_POINT('Ctrl Pts',(12.5175897865895,12.2294774556221,98.4717229246488));
#30207=CARTESIAN_POINT('Ctrl Pts',(12.5267717721302,12.2200650149237,98.4764616066469));
#30208=CARTESIAN_POINT('Origin',(7.52738542590446,15.2389652387019,98.280871015943));
#30209=CARTESIAN_POINT('Origin',(12.1688640072122,11.8709203002116,100.));
#30210=CARTESIAN_POINT('Ctrl Pts',(12.1768261106186,12.3708569011015,0.5));
#30211=CARTESIAN_POINT('Ctrl Pts',(12.1778203104535,12.37084106725,0.498951748855235));
#30212=CARTESIAN_POINT('Ctrl Pts',(12.1788144663232,12.3708222676705,0.497903494267714));
#30213=CARTESIAN_POINT('Ctrl Pts',(12.2687615400859,12.3688529339418,0.403057585612054));
#30214=CARTESIAN_POINT('Ctrl Pts',(12.3562405730693,12.3432084553889,0.310543821638481));
#30215=CARTESIAN_POINT('Ctrl Pts',(12.467152867614,12.2742120695516,0.195519413317804));
#30216=CARTESIAN_POINT('Ctrl Pts',(12.4986401261746,12.2489027263458,0.1632025467695));
#30217=CARTESIAN_POINT('Ctrl Pts',(12.5267717721302,12.2200650149237,0.134720657333169));
#30218=CARTESIAN_POINT('Origin',(7.52953032547043,15.2415935216047,100.));
#30219=CARTESIAN_POINT('Ctrl Pts',(7.75098709974897,15.6898756840048,0.134720657333167));
#30220=CARTESIAN_POINT('Ctrl Pts',(7.78710654979212,15.6720322417129,0.163202546769546));
#30221=CARTESIAN_POINT('Ctrl Pts',(7.82090726357265,15.6499070964456,0.195519413317857));
#30222=CARTESIAN_POINT('Ctrl Pts',(7.92080050982121,15.5657442917577,0.310543821635948));
#30223=CARTESIAN_POINT('Ctrl Pts',(7.97222236610058,15.4904713670851,0.403057585608259));
#30224=CARTESIAN_POINT('Ctrl Pts',(8.00189048816382,15.4055351740487,0.4979034942676));
#30225=CARTESIAN_POINT('Ctrl Pts',(8.00221557868522,15.4045954850201,0.498951748855171));
#30226=CARTESIAN_POINT('Ctrl Pts',(8.00253786221767,15.4036548377177,0.5));
#30227=CARTESIAN_POINT('Origin',(12.2482946431511,16.8583313034371,0.5));
#30228=CARTESIAN_POINT('Ctrl Pts',(17.3143275674006,2.71461308502431,98.1029310400785));
#30229=CARTESIAN_POINT('Ctrl Pts',(17.4636977396689,2.61423858413124,98.3435819247051));
#30230=CARTESIAN_POINT('Ctrl Pts',(17.3857742403068,2.34690286052699,98.4565369100693));
#30231=CARTESIAN_POINT('Ctrl Pts',(17.1296512858619,2.83873298501121,98.287884067932));
#30232=CARTESIAN_POINT('Ctrl Pts',(17.2651608223732,2.73703317193548,98.5214982032519));
#30233=CARTESIAN_POINT('Ctrl Pts',(17.1800764226929,2.48819271337626,98.641483434387));
#30234=CARTESIAN_POINT('Ctrl Pts',(16.9451136614474,2.98310069417807,98.4673409000312));
#30235=CARTESIAN_POINT('Ctrl Pts',(17.0639661472453,2.88326764438849,98.6966806272835));
#30236=CARTESIAN_POINT('Ctrl Pts',(16.9743943558493,2.65255720272719,98.8209468545489));
#30237=CARTESIAN_POINT('Ctrl Pts',(16.5997101391575,3.30279942760431,98.786605947879));
#30238=CARTESIAN_POINT('Ctrl Pts',(16.6878268341946,3.21163443205183,99.007927768118));
#30239=CARTESIAN_POINT('Ctrl Pts',(16.5890378089607,3.01654651232656,99.1402125820164));
#30240=CARTESIAN_POINT('Ctrl Pts',(16.4374762686561,3.47698561123582,98.9284804941304));
#30241=CARTESIAN_POINT('Ctrl Pts',(16.5106768516082,3.39212226298075,99.1468659074354));
#30242=CARTESIAN_POINT('Ctrl Pts',(16.4078485131262,3.21487371577908,99.28208744884));
#30243=CARTESIAN_POINT('Ctrl Pts',(16.2075579278768,3.77068327953469,99.1108598027282));
#30244=CARTESIAN_POINT('Ctrl Pts',(16.2598042688104,3.69971142057243,99.3254864613232));
#30245=CARTESIAN_POINT('Ctrl Pts',(16.1506324221162,3.54922452427067,99.4644671720462));
#30246=CARTESIAN_POINT('Ctrl Pts',(16.1328338869385,3.87465067488052,99.1667281040791));
#30247=CARTESIAN_POINT('Ctrl Pts',(16.1785346664591,3.80861210815899,99.3801095631261));
#30248=CARTESIAN_POINT('Ctrl Pts',(16.0669575425481,3.66757422893044,99.5203355960162));
#30249=CARTESIAN_POINT('Ctrl Pts',(15.9919866048144,4.08994756745576,99.2638527346785));
#30250=CARTESIAN_POINT('Ctrl Pts',(16.0257056636235,4.03466861210541,99.4749661095219));
#30251=CARTESIAN_POINT('Ctrl Pts',(15.9090517391356,3.91261572849131,99.6174604374823));
#30252=CARTESIAN_POINT('Ctrl Pts',(15.9254898327247,4.20166713029547,99.305439932531));
#30253=CARTESIAN_POINT('Ctrl Pts',(15.953587399343,4.15233969324182,99.5156582141651));
#30254=CARTESIAN_POINT('Ctrl Pts',(15.8344036945523,4.03975173211327,99.6590477275202));
#30255=CARTESIAN_POINT('Ctrl Pts',(15.7386039884752,4.55006349017908,99.4071746058889));
#30256=CARTESIAN_POINT('Ctrl Pts',(15.7519852189442,4.51914563857043,99.6148745113223));
#30257=CARTESIAN_POINT('Ctrl Pts',(15.6242698911525,4.43612723332498,99.7607826165547));
#30258=CARTESIAN_POINT('Ctrl Pts',(15.6300705661688,4.80379339451689,99.4435386777496));
#30259=CARTESIAN_POINT('Ctrl Pts',(15.6349263242122,4.78871307695064,99.6506668510312));
#30260=CARTESIAN_POINT('Ctrl Pts',(15.5017253412089,4.72466850699764,99.7971467765045));
#30261=CARTESIAN_POINT('Ctrl Pts',(15.5059824861585,5.18799157661501,99.442502700397));
#30262=CARTESIAN_POINT('Ctrl Pts',(15.5033523953774,5.19622875259004,99.6496543232893));
#30263=CARTESIAN_POINT('Ctrl Pts',(15.3607119866152,5.16119508122743,99.7961107967628));
#30264=CARTESIAN_POINT('Ctrl Pts',(15.4705223787628,5.31743764272476,99.4333242900205));
#30265=CARTESIAN_POINT('Ctrl Pts',(15.466074874266,5.333778711027,99.6406660872408));
#30266=CARTESIAN_POINT('Ctrl Pts',(15.3202268375056,5.30821065016257,99.7869323657971));
#30267=CARTESIAN_POINT('Ctrl Pts',(15.4112870235324,5.57906517882989,99.3975703058088));
#30268=CARTESIAN_POINT('Ctrl Pts',(15.4046994857704,5.61160402086349,99.605723827768));
#30269=CARTESIAN_POINT('Ctrl Pts',(15.2521751775211,5.6051982497642,99.751178303339));
#30270=CARTESIAN_POINT('Ctrl Pts',(15.3873774999491,5.71249818528157,99.3706193994188));
#30271=CARTESIAN_POINT('Ctrl Pts',(15.3804432938943,5.75346933726163,99.5793392014518));
#30272=CARTESIAN_POINT('Ctrl Pts',(15.2244484235508,5.75658897920106,99.7242273368567));
#30273=CARTESIAN_POINT('Ctrl Pts',(15.3346696945248,6.10616299653768,99.2668124456041));
#30274=CARTESIAN_POINT('Ctrl Pts',(15.3287678592424,6.17236078267489,99.4777222783444));
#30275=CARTESIAN_POINT('Ctrl Pts',(15.1624256089297,6.20298061454619,99.6204201490477));
#30276=CARTESIAN_POINT('Ctrl Pts',(15.3240667024475,6.35937968875434,99.1683014346687));
#30277=CARTESIAN_POINT('Ctrl Pts',(15.3219320743537,6.4418547297802,99.3809681438969));
#30278=CARTESIAN_POINT('Ctrl Pts',(15.1483769580277,6.48977650021848,99.5219089068378));
#30279=CARTESIAN_POINT('Ctrl Pts',(15.3423230787144,6.8517981468714,98.9266153300884));
#30280=CARTESIAN_POINT('Ctrl Pts',(15.3517693972099,6.96362633911536,99.1450562468822));
#30281=CARTESIAN_POINT('Ctrl Pts',(15.1643067184422,7.04682949241163,99.2802222813138));
#30282=CARTESIAN_POINT('Ctrl Pts',(15.3719403060826,7.09247220631589,98.7818489409675));
#30283=CARTESIAN_POINT('Ctrl Pts',(15.3899215235328,7.21841417521577,99.0032991843689));
#30284=CARTESIAN_POINT('Ctrl Pts',(15.1951156833261,7.31874252774784,99.1354555654036));
#30285=CARTESIAN_POINT('Ctrl Pts',(15.4635565836047,7.55131386473068,98.4637529208263));
#30286=CARTESIAN_POINT('Ctrl Pts',(15.5012645827149,7.70215187781829,98.6931970174467));
#30287=CARTESIAN_POINT('Ctrl Pts',(15.2930580254608,7.83652577457457,98.817358868105));
#30288=CARTESIAN_POINT('Ctrl Pts',(15.5265390080798,7.771324565253,98.288422358758));
#30289=CARTESIAN_POINT('Ctrl Pts',(15.5763509023311,7.93321211466989,98.5220290043357));
#30290=CARTESIAN_POINT('Ctrl Pts',(15.3612680514934,8.08445864294548,98.6420342839988));
#30291=CARTESIAN_POINT('Ctrl Pts',(15.6032141429119,7.98099597100254,98.1028819381727));
#30292=CARTESIAN_POINT('Ctrl Pts',(15.6650624954954,8.15000252629558,98.3435328809189));
#30293=CARTESIAN_POINT('Ctrl Pts',(15.4448833406996,8.32048399603211,98.4564865387793));
#30294=CARTESIAN_POINT('Ctrl Pts',(17.1226665060507,2.85087466017704,98.292893219028));
#30295=CARTESIAN_POINT('Ctrl Pts',(17.1491844558261,2.83095542391965,98.3104738971227));
#30296=CARTESIAN_POINT('Ctrl Pts',(17.1736001786239,2.80849354482898,98.3279440199826));
#30297=CARTESIAN_POINT('Ctrl Pts',(17.1956168298849,2.78379335217174,98.3450378047574));
#30298=CARTESIAN_POINT('Ctrl Pts',(17.2156466199956,2.76132219301346,98.3605889854151));
#30299=CARTESIAN_POINT('Ctrl Pts',(17.2336921685704,2.73699581706788,98.37582868731));
#30300=CARTESIAN_POINT('Ctrl Pts',(17.2494951641239,2.71102785622515,98.3905567849746));
#30301=CARTESIAN_POINT('Ctrl Pts',(17.2639409440128,2.68729011326205,98.4040199829058));
#30302=CARTESIAN_POINT('Ctrl Pts',(17.2765129069447,2.66217890823152,98.4170556796967));
#30303=CARTESIAN_POINT('Ctrl Pts',(17.2869749123056,2.63587291044608,98.4295110106904));
#30304=CARTESIAN_POINT('Ctrl Pts',(17.2964430397672,2.61206595074306,98.4407831002524));
#30305=CARTESIAN_POINT('Ctrl Pts',(17.3041825760947,2.58727949049788,98.4515798544512));
#30306=CARTESIAN_POINT('Ctrl Pts',(17.3099886550643,2.56167649685877,98.4617879668562));
#30307=CARTESIAN_POINT('Ctrl Pts',(17.3128548068259,2.54903766337002,98.4668271679255));
#30308=CARTESIAN_POINT('Ctrl Pts',(17.3152493576036,2.53620042325289,98.4717229246001));
#30309=CARTESIAN_POINT('Ctrl Pts',(17.3171452461371,2.52318856294818,98.4764616066469));
#30310=CARTESIAN_POINT('Origin',(15.0469618583329,7.90408080223432,98.2808650734389));
#30311=CARTESIAN_POINT('Origin',(16.822369667676,2.45109746114966,100.));
#30312=CARTESIAN_POINT('Ctrl Pts',(17.122666505727,2.85087466042014,0.5));
#30313=CARTESIAN_POINT('Ctrl Pts',(17.1234615233843,2.85027747456484,0.498951748855993));
#30314=CARTESIAN_POINT('Ctrl Pts',(17.1242547622613,2.84967791522767,0.497903494266448));
#30315=CARTESIAN_POINT('Ctrl Pts',(17.1958659280646,2.79521512743788,0.403057585878129));
#30316=CARTESIAN_POINT('Ctrl Pts',(17.2515645061738,2.72304942307884,0.31054382181288));
#30317=CARTESIAN_POINT('Ctrl Pts',(17.3007393793639,2.60203756316583,0.195519413314306));
#30318=CARTESIAN_POINT('Ctrl Pts',(17.3113366479633,2.56305412818084,0.163202546767945));
#30319=CARTESIAN_POINT('Ctrl Pts',(17.3171452461371,2.52318856294818,0.134720657333154));
#30320=CARTESIAN_POINT('Origin',(15.0503018864028,7.90496129833282,100.));
#30321=CARTESIAN_POINT('Ctrl Pts',(15.4929578242382,8.13746016004849,0.134720657333155));
#30322=CARTESIAN_POINT('Ctrl Pts',(15.5116909609202,8.10179403194187,0.163202546767978));
#30323=CARTESIAN_POINT('Ctrl Pts',(15.5260314786972,8.06402685234251,0.195519413314386));
#30324=CARTESIAN_POINT('Ctrl Pts',(15.557377157194,7.93722193592991,0.310543821792654));
#30325=CARTESIAN_POINT('Ctrl Pts',(15.5547339976961,7.84609985190388,0.403057585847384));
#30326=CARTESIAN_POINT('Ctrl Pts',(15.5288117710301,7.75994654384289,0.497903494266064));
#30327=CARTESIAN_POINT('Ctrl Pts',(15.5285224394342,7.75899523603605,0.498951748855763));
#30328=CARTESIAN_POINT('Ctrl Pts',(15.5282302736771,7.75804480287584,0.5));
#30329=CARTESIAN_POINT('Origin',(19.8181570368417,6.43930956430664,0.5));
#30330=CARTESIAN_POINT('Ctrl Pts',(17.3656407514415,-2.36084587016586,98.4746163542476));
#30331=CARTESIAN_POINT('Ctrl Pts',(17.4440265737737,-2.62644363351055,98.3611663178014));
#30332=CARTESIAN_POINT('Ctrl Pts',(17.2962665385767,-2.72681679293049,98.1210629636544));
#30333=CARTESIAN_POINT('Ctrl Pts',(16.9690963360069,-2.63613637636299,98.8304618827584));
#30334=CARTESIAN_POINT('Ctrl Pts',(17.0649442889613,-2.86366294455655,98.7002300650184));
#30335=CARTESIAN_POINT('Ctrl Pts',(16.9402678976059,-2.96864610960458,98.4769098403642));
#30336=CARTESIAN_POINT('Ctrl Pts',(16.579352085484,-2.99263453637889,99.1602382875981));
#30337=CARTESIAN_POINT('Ctrl Pts',(16.6807262887858,-3.184238518665,99.0255494138259));
#30338=CARTESIAN_POINT('Ctrl Pts',(16.5907862689851,-3.28173103979709,98.8066848982746));
#30339=CARTESIAN_POINT('Ctrl Pts',(16.06825893873,-3.65601467024647,99.5229830380903));
#30340=CARTESIAN_POINT('Ctrl Pts',(16.1805213417482,-3.79657900263654,99.3820315078356));
#30341=CARTESIAN_POINT('Ctrl Pts',(16.1339186653847,-3.8644611469686,99.1694296468622));
#30342=CARTESIAN_POINT('Ctrl Pts',(15.9074663690947,-3.90241128133998,99.6234913693261));
#30343=CARTESIAN_POINT('Ctrl Pts',(16.0241813784631,-4.02429095582515,99.480742609552));
#30344=CARTESIAN_POINT('Ctrl Pts',(15.9904645360934,-4.08092818635296,99.2699379792835));
#30345=CARTESIAN_POINT('Ctrl Pts',(15.6245522069462,-4.43521068708324,99.7608048122965));
#30346=CARTESIAN_POINT('Ctrl Pts',(15.7522284341321,-4.51825273440788,99.6149071958598));
#30347=CARTESIAN_POINT('Ctrl Pts',(15.738838796464,-4.54924202639042,99.4072514211525));
#30348=CARTESIAN_POINT('Ctrl Pts',(15.5044462303209,-4.71763971050874,99.7966027452518));
#30349=CARTESIAN_POINT('Ctrl Pts',(15.637469741455,-4.7821404952998,99.6501526042829));
#30350=CARTESIAN_POINT('Ctrl Pts',(15.6324601989204,-4.79760023853972,99.4430493547679));
#30351=CARTESIAN_POINT('Ctrl Pts',(15.3625803721861,-5.15483225994623,99.79636776423));
#30352=CARTESIAN_POINT('Ctrl Pts',(15.5050490252728,-5.19027311193596,99.6499229371967));
#30353=CARTESIAN_POINT('Ctrl Pts',(15.5076044740505,-5.18238705961208,99.442814373582));
#30354=CARTESIAN_POINT('Ctrl Pts',(15.3211549463132,-5.30458937654577,99.7872514480855));
#30355=CARTESIAN_POINT('Ctrl Pts',(15.4668882655262,-5.33038662434131,99.6409952531274));
#30356=CARTESIAN_POINT('Ctrl Pts',(15.4713150290528,-5.31424796399517,99.4336980572382));
#30357=CARTESIAN_POINT('Ctrl Pts',(15.2524387792612,-5.60380285207576,99.7514230350794));
#30358=CARTESIAN_POINT('Ctrl Pts',(15.4048955461524,-5.61029467639232,99.6059800049562));
#30359=CARTESIAN_POINT('Ctrl Pts',(15.4114951404923,-5.57783990353114,99.3978696447402));
#30360=CARTESIAN_POINT('Ctrl Pts',(15.225232210421,-5.75229303761941,99.7250021223377));
#30361=CARTESIAN_POINT('Ctrl Pts',(15.3810929371293,-5.74943839640601,99.580115086457));
#30362=CARTESIAN_POINT('Ctrl Pts',(15.3880333336981,-5.70871875235854,99.3714487314956));
#30363=CARTESIAN_POINT('Ctrl Pts',(15.1632690619364,-6.19474020261596,99.6227146850679));
#30364=CARTESIAN_POINT('Ctrl Pts',(15.3293788683914,-6.16461669902609,99.4799874409064));
#30365=CARTESIAN_POINT('Ctrl Pts',(15.335349988799,-6.09890683169226,99.2691612949723));
#30366=CARTESIAN_POINT('Ctrl Pts',(15.1483715649769,-6.48916504798079,99.522165658859));
#30367=CARTESIAN_POINT('Ctrl Pts',(15.3218719375042,-6.44129651453827,99.3812294188918));
#30368=CARTESIAN_POINT('Ctrl Pts',(15.3240366258068,-6.35885837698108,99.1686122675856));
#30369=CARTESIAN_POINT('Ctrl Pts',(15.1643710385717,-7.047829358343,99.279753346815));
#30370=CARTESIAN_POINT('Ctrl Pts',(15.3518153879027,-6.96458278973335,99.1446071116389));
#30371=CARTESIAN_POINT('Ctrl Pts',(15.3423676517735,-6.8527101484055,98.9261999569019));
#30372=CARTESIAN_POINT('Ctrl Pts',(15.1944125118879,-7.31378505933127,99.138252154167));
#30373=CARTESIAN_POINT('Ctrl Pts',(15.3890461250774,-7.21380562024091,99.0060308920462));
#30374=CARTESIAN_POINT('Ctrl Pts',(15.371253945164,-7.08811389017374,98.7846987631153));
#30375=CARTESIAN_POINT('Ctrl Pts',(15.290724890162,-7.8251126253835,98.8245648611892));
#30376=CARTESIAN_POINT('Ctrl Pts',(15.4985537486393,-7.69138492458423,98.7003130263028));
#30377=CARTESIAN_POINT('Ctrl Pts',(15.461363297308,-7.54123627293857,98.4710114710543));
#30378=CARTESIAN_POINT('Ctrl Pts',(15.3574639152262,-8.06994831582715,98.6521093612505));
#30379=CARTESIAN_POINT('Ctrl Pts',(15.5720250893885,-7.91951631844379,98.5320184901569));
#30380=CARTESIAN_POINT('Ctrl Pts',(15.5230000877303,-7.75847929885463,98.2985618527043));
#30381=CARTESIAN_POINT('Ctrl Pts',(15.4367365239838,-8.29721036780905,98.4746887503082));
#30382=CARTESIAN_POINT('Ctrl Pts',(15.6562640576654,-8.12841791648205,98.3612367156073));
#30383=CARTESIAN_POINT('Ctrl Pts',(15.5957265901482,-7.96036688919461,98.1211353597149));
#30384=CARTESIAN_POINT('Ctrl Pts',(15.5282302741409,-7.75804480438455,98.2928932196501));
#30385=CARTESIAN_POINT('Ctrl Pts',(15.5379755127592,-7.78974666478008,98.3104738976971));
#30386=CARTESIAN_POINT('Ctrl Pts',(15.5445254860806,-7.82226990841396,98.3279440205092));
#30387=CARTESIAN_POINT('Ctrl Pts',(15.5478189220675,-7.8551938468868,98.3450378052369));
#30388=CARTESIAN_POINT('Ctrl Pts',(15.5508151466442,-7.88514661172166,98.3605889858622));
#30389=CARTESIAN_POINT('Ctrl Pts',(15.5511156170379,-7.91543397054887,98.3758286877249));
#30390=CARTESIAN_POINT('Ctrl Pts',(15.548636924542,-7.94573125985883,98.3905567853577));
#30391=CARTESIAN_POINT('Ctrl Pts',(15.5463711106901,-7.97342651366893,98.4040199832666));
#30392=CARTESIAN_POINT('Ctrl Pts',(15.5417820463325,-8.00113151965715,98.4170556800349));
#30393=CARTESIAN_POINT('Ctrl Pts',(15.5347837088864,-8.02856293134369,98.429511011006));
#30394=CARTESIAN_POINT('Ctrl Pts',(15.5284502050597,-8.0533883919943,98.4407831005523));
#30395=CARTESIAN_POINT('Ctrl Pts',(15.5201425056581,-8.07799024485183,98.451579854735));
#30396=CARTESIAN_POINT('Ctrl Pts',(15.5097906601113,-8.10211622937918,98.4617879671231));
#30397=CARTESIAN_POINT('Ctrl Pts',(15.5046805057368,-8.11402594198207,98.4668271680985));
#30398=CARTESIAN_POINT('Ctrl Pts',(15.4990721976791,-8.12581896881945,98.471722924684));
#30399=CARTESIAN_POINT('Ctrl Pts',(15.4929578242382,-8.13746016004849,98.4764616066469));
#30400=CARTESIAN_POINT('Ctrl Pts',(17.3171452461371,-2.52318856294819,98.4764616066469));
#30401=CARTESIAN_POINT('Ctrl Pts',(17.3132089417597,-2.55020420325235,98.4666230035039));
#30402=CARTESIAN_POINT('Ctrl Pts',(17.307113237115,-2.57652769355605,98.4560730110188));
#30403=CARTESIAN_POINT('Ctrl Pts',(17.2990811363586,-2.6019158142319,98.4449543865012));
#30404=CARTESIAN_POINT('Ctrl Pts',(17.2902502712352,-2.62982869483757,98.4327300536087));
#30405=CARTESIAN_POINT('Ctrl Pts',(17.2790794105449,-2.65661115931836,98.4198183681966));
#30406=CARTESIAN_POINT('Ctrl Pts',(17.2658576960617,-2.68200516712457,98.4064090535635));
#30407=CARTESIAN_POINT('Ctrl Pts',(17.2516730980635,-2.70924851689978,98.392023193262));
#30408=CARTESIAN_POINT('Ctrl Pts',(17.2351284858505,-2.73489473602574,98.3770645838946));
#30409=CARTESIAN_POINT('Ctrl Pts',(17.2165633719675,-2.75868699851548,98.3617674910173));
#30410=CARTESIAN_POINT('Ctrl Pts',(17.194826807983,-2.78654365693436,98.3438572190847));
#30411=CARTESIAN_POINT('Ctrl Pts',(17.1703205947608,-2.81185976444954,98.3254829406478));
#30412=CARTESIAN_POINT('Ctrl Pts',(17.1435596961152,-2.83429057908266,98.307020656073));
#30413=CARTESIAN_POINT('Ctrl Pts',(17.1367405895733,-2.84000631071152,98.302316169606));
#30414=CARTESIAN_POINT('Ctrl Pts',(17.1297749579395,-2.84553494378639,98.297605968793));
#30415=CARTESIAN_POINT('Ctrl Pts',(17.1226711151597,-2.85087119795487,98.2928962747547));
#30416=CARTESIAN_POINT('Origin',(15.0503018864028,-7.90496129833282,100.));
#30417=CARTESIAN_POINT('Ctrl Pts',(15.5282302736771,-7.75804480287558,0.49999999999973));
#30418=CARTESIAN_POINT('Ctrl Pts',(15.5285224394342,-7.75899523603614,0.498951748855111));
#30419=CARTESIAN_POINT('Ctrl Pts',(15.5288117710303,-7.75994654384333,0.497903494267013));
#30420=CARTESIAN_POINT('Ctrl Pts',(15.5547339977176,-7.84609985197566,0.403057585737619));
#30421=CARTESIAN_POINT('Ctrl Pts',(15.5573771571738,-7.93722193600944,0.310543821720739));
#30422=CARTESIAN_POINT('Ctrl Pts',(15.526031478698,-8.06402685234064,0.195519413315996));
#30423=CARTESIAN_POINT('Ctrl Pts',(15.5116909609207,-8.10179403194099,0.16320254676869));
#30424=CARTESIAN_POINT('Ctrl Pts',(15.4929578242382,-8.13746016004849,0.134720657333159));
#30425=CARTESIAN_POINT('Origin',(16.822369667676,-2.45109746114967,100.));
#30426=CARTESIAN_POINT('Ctrl Pts',(17.3171452461371,-2.52318856294818,0.134720657333158));
#30427=CARTESIAN_POINT('Ctrl Pts',(17.3113366479632,-2.56305412818187,0.163202546768687));
#30428=CARTESIAN_POINT('Ctrl Pts',(17.3007393793634,-2.6020375631678,0.195519413315945));
#30429=CARTESIAN_POINT('Ctrl Pts',(17.2515645062122,-2.72304942298316,0.310543821722463));
#30430=CARTESIAN_POINT('Ctrl Pts',(17.1958659281393,-2.79521512738078,0.403057585740282));
#30431=CARTESIAN_POINT('Ctrl Pts',(17.1242547622625,-2.84967791522681,0.497903494266715));
#30432=CARTESIAN_POINT('Ctrl Pts',(17.1234615233847,-2.85027747456458,0.498951748855534));
#30433=CARTESIAN_POINT('Ctrl Pts',(17.122666505727,-2.85087466042014,0.5));
#30434=CARTESIAN_POINT('Origin',(19.8181570368417,-6.43930956430665,0.5));
#30435=CARTESIAN_POINT('Ctrl Pts',(7.93217192832153,-15.6280424815125,98.1029310403445));
#30436=CARTESIAN_POINT('Ctrl Pts',(7.88286802685372,-15.8011193837442,98.3435819249637));
#30437=CARTESIAN_POINT('Ctrl Pts',(7.6045369593389,-15.8096210136862,98.4565369103351));
#30438=CARTESIAN_POINT('Ctrl Pts',(7.99314885854194,-15.4140497422101,98.2878840681048));
#30439=CARTESIAN_POINT('Ctrl Pts',(7.93830133828976,-15.5743539404758,98.5214982034216));
#30440=CARTESIAN_POINT('Ctrl Pts',(7.67534747321689,-15.5703297983009,98.6414834345591));
#30441=CARTESIAN_POINT('Ctrl Pts',(8.07342544701253,-15.1939319565459,98.4673409001091));
#30442=CARTESIAN_POINT('Ctrl Pts',(8.01520601240404,-15.3378174966169,98.6966806273606));
#30443=CARTESIAN_POINT('Ctrl Pts',(7.76810813773369,-15.3239231079837,98.8209468546265));
#30444=CARTESIAN_POINT('Ctrl Pts',(8.27074145233723,-14.766641344314,98.7866059478792));
#30445=CARTESIAN_POINT('Ctrl Pts',(8.21126794551389,-14.8786168342413,99.007927768118));
#30446=CARTESIAN_POINT('Ctrl Pts',(7.99520082055391,-14.8449483706468,99.1402125820164));
#30447=CARTESIAN_POINT('Ctrl Pts',(8.38626933427988,-14.5585212736834,98.9284804941306));
#30448=CARTESIAN_POINT('Ctrl Pts',(8.32817971805786,-14.6543633819064,99.1468659074354));
#30449=CARTESIAN_POINT('Ctrl Pts',(8.12783062814372,-14.6113406338471,99.2820874488401));
#30450=CARTESIAN_POINT('Ctrl Pts',(8.59454374091697,-14.2490983667568,99.1108598027283));
#30451=CARTESIAN_POINT('Ctrl Pts',(8.54319049921963,-14.3207191002961,99.3254864613231));
#30452=CARTESIAN_POINT('Ctrl Pts',(8.3663329999392,-14.2633935124896,99.464467172046));
#30453=CARTESIAN_POINT('Ctrl Pts',(8.67033161120457,-14.1459038886756,99.1667281040793));
#30454=CARTESIAN_POINT('Ctrl Pts',(8.62164751952522,-14.2097749522395,99.3801095631261));
#30455=CARTESIAN_POINT('Ctrl Pts',(8.45303329796877,-14.1472419030066,99.5203355960163));
#30456=CARTESIAN_POINT('Ctrl Pts',(8.83156692003841,-13.9454197645673,99.2638527346786));
#30457=CARTESIAN_POINT('Ctrl Pts',(8.78941327154489,-13.9945706318056,99.4749661095218));
#30458=CARTESIAN_POINT('Ctrl Pts',(8.63728603612383,-13.9213425720194,99.617460437482));
#30459=CARTESIAN_POINT('Ctrl Pts',(8.91726990562806,-13.8476543326371,99.30543993253));
#30460=CARTESIAN_POINT('Ctrl Pts',(8.87903935077169,-13.8896197227996,99.5156582141639));
#30461=CARTESIAN_POINT('Ctrl Pts',(8.73513204645164,-13.8110608770739,99.6590477275195));
#30462=CARTESIAN_POINT('Ctrl Pts',(9.19086363206755,-13.562254936678,99.4071746058911));
#30463=CARTESIAN_POINT('Ctrl Pts',(9.16559403544582,-13.5845353846886,99.6148745113244));
#30464=CARTESIAN_POINT('Ctrl Pts',(9.04717263343429,-13.4887249880271,99.7607826165557));
#30465=CARTESIAN_POINT('Ctrl Pts',(9.39863643901659,-13.3806266657362,99.4435386777497));
#30466=CARTESIAN_POINT('Ctrl Pts',(9.38579471648297,-13.3899048404733,99.6506668510312));
#30467=CARTESIAN_POINT('Ctrl Pts',(9.28372334348073,-13.2830140381241,99.7971467765045));
#30468=CARTESIAN_POINT('Ctrl Pts',(9.72568529812741,-13.1438881211714,99.4425027003972));
#30469=CARTESIAN_POINT('Ctrl Pts',(9.73270657526636,-13.1388413288337,99.6496543232893));
#30470=CARTESIAN_POINT('Ctrl Pts',(9.6553092634351,-13.0140082384199,99.7961107967625));
#30471=CARTESIAN_POINT('Ctrl Pts',(9.83783804700212,-13.0701625206813,99.4333242900206));
#30472=CARTESIAN_POINT('Ctrl Pts',(9.85200497202214,-13.0608830247368,99.6406660872408));
#30473=CARTESIAN_POINT('Ctrl Pts',(9.78261877917292,-12.9300742643074,99.786932365797));
#30474=CARTESIAN_POINT('Ctrl Pts',(10.0683558886232,-12.9329789952414,99.3975703058089));
#30475=CARTESIAN_POINT('Ctrl Pts',(10.0972665052523,-12.9166588193609,99.605723827768));
#30476=CARTESIAN_POINT('Ctrl Pts',(10.0440416516022,-12.7735790742389,99.7511783033389));
#30477=CARTESIAN_POINT('Ctrl Pts',(10.1878697697833,-12.869006620432,99.3706193994189));
#30478=CARTESIAN_POINT('Ctrl Pts',(10.2246928633403,-12.8497510163372,99.5793392014518));
#30479=CARTESIAN_POINT('Ctrl Pts',(10.1794547531642,-12.7004270560129,99.7242273368565));
#30480=CARTESIAN_POINT('Ctrl Pts',(10.5459796461522,-12.697229401858,99.2668124456042));
#30481=CARTESIAN_POINT('Ctrl Pts',(10.6071137146224,-12.6711601820482,99.4777222783443));
#30482=CARTESIAN_POINT('Ctrl Pts',(10.5848323230218,-12.5034972525401,99.6204201490476));
#30483=CARTESIAN_POINT('Ctrl Pts',(10.7835265265762,-12.6088970959964,99.1683014346688));
#30484=CARTESIAN_POINT('Ctrl Pts',(10.8613053154178,-12.5813807547492,99.3809681438969));
#30485=CARTESIAN_POINT('Ctrl Pts',(10.8532501470603,-12.4015113889649,99.5219089068378));
#30486=CARTESIAN_POINT('Ctrl Pts',(11.2574858404352,-12.4740942697067,98.9266153300885));
#30487=CARTESIAN_POINT('Ctrl Pts',(11.3667598443235,-12.4485214406132,99.1450562468822));
#30488=CARTESIAN_POINT('Ctrl Pts',(11.3879615918918,-12.2445226500553,99.2802222813136));
#30489=CARTESIAN_POINT('Ctrl Pts',(11.4955326995555,-12.4278895523164,98.7818489409676));
#30490=CARTESIAN_POINT('Ctrl Pts',(11.6208671315241,-12.406072497649,99.0032991843688));
#30491=CARTESIAN_POINT('Ctrl Pts',(11.6560867497417,-12.1897979679578,99.1354555654035));
#30492=CARTESIAN_POINT('Ctrl Pts',(11.9602280353417,-12.3732319398884,98.4637529209039));
#30493=CARTESIAN_POINT('Ctrl Pts',(12.1153359231333,-12.3624828687134,98.6931970175235));
#30494=CARTESIAN_POINT('Ctrl Pts',(12.1787937287267,-12.1229428480096,98.8173588681825));
#30495=CARTESIAN_POINT('Ctrl Pts',(12.1889332851312,-12.3651447396863,98.2884223589262));
#30496=CARTESIAN_POINT('Ctrl Pts',(12.3582902157402,-12.362492662348,98.522029004501));
#30497=CARTESIAN_POINT('Ctrl Pts',(12.4356699559058,-12.1111989679491,98.6420342841671));
#30498=CARTESIAN_POINT('Ctrl Pts',(12.412036561458,-12.3732750986756,98.1028819384397));
#30499=CARTESIAN_POINT('Ctrl Pts',(12.5918835391696,-12.3798704796622,98.3435328811783));
#30500=CARTESIAN_POINT('Ctrl Pts',(12.6859819512106,-12.1177859883829,98.456486539046));
#30501=CARTESIAN_POINT('Ctrl Pts',(8.00253786208648,-15.4036548381007,98.292893219028));
#30502=CARTESIAN_POINT('Ctrl Pts',(7.99178803981921,-15.4350302894399,98.3104738970446));
#30503=CARTESIAN_POINT('Ctrl Pts',(7.97797039667762,-15.4651921239651,98.3279440198334));
#30504=CARTESIAN_POINT('Ctrl Pts',(7.9612826369793,-15.4937639828144,98.3450378045448));
#30505=CARTESIAN_POINT('Ctrl Pts',(7.94610084020688,-15.5197574152645,98.3605889851856));
#30506=CARTESIAN_POINT('Ctrl Pts',(7.92854146306982,-15.54443701539,98.3758286870684));
#30507=CARTESIAN_POINT('Ctrl Pts',(7.90872785893013,-15.5674910984875,98.3905567847244));
#30508=CARTESIAN_POINT('Ctrl Pts',(7.89061591531714,-15.5885652175708,98.404019982656));
#30509=CARTESIAN_POINT('Ctrl Pts',(7.87061869037307,-15.6082816539495,98.4170556794497));
#30510=CARTESIAN_POINT('Ctrl Pts',(7.84883313724825,-15.626360612701,98.4295110104475));
#30511=CARTESIAN_POINT('Ctrl Pts',(7.82911718541249,-15.6427220921615,98.4407831000128));
#30512=CARTESIAN_POINT('Ctrl Pts',(7.80793550916779,-15.6577422660767,98.4515798542159));
#30513=CARTESIAN_POINT('Ctrl Pts',(7.78537979233681,-15.6711759354721,98.4617879666255));
#30514=CARTESIAN_POINT('Ctrl Pts',(7.77424523683315,-15.677807422231,98.4668271677764));
#30515=CARTESIAN_POINT('Ctrl Pts',(7.76277625268364,-15.6840517008099,98.4717229245282));
#30516=CARTESIAN_POINT('Ctrl Pts',(7.75098709974897,-15.6898756840048,98.4764616066469));
#30517=CARTESIAN_POINT('Origin',(12.1669944796941,-11.8680158320171,98.2808650733939));
#30518=CARTESIAN_POINT('Origin',(7.52953032547043,-15.2415935216047,100.));
#30519=CARTESIAN_POINT('Ctrl Pts',(8.00253786221767,-15.4036548377177,0.5));
#30520=CARTESIAN_POINT('Ctrl Pts',(8.00221557868522,-15.4045954850201,0.498951748855171));
#30521=CARTESIAN_POINT('Ctrl Pts',(8.00189048816382,-15.4055351740487,0.4979034942676));
#30522=CARTESIAN_POINT('Ctrl Pts',(7.97222236610058,-15.4904713670851,0.403057585608257));
#30523=CARTESIAN_POINT('Ctrl Pts',(7.92080050982121,-15.5657442917577,0.310543821635946));
#30524=CARTESIAN_POINT('Ctrl Pts',(7.82090726357263,-15.6499070964456,0.19551941331783));
#30525=CARTESIAN_POINT('Ctrl Pts',(7.78710654979209,-15.6720322417129,0.163202546769525));
#30526=CARTESIAN_POINT('Ctrl Pts',(7.75098709974897,-15.6898756840048,0.134720657333167));
#30527=CARTESIAN_POINT('Origin',(12.1688640072122,-11.8709203002116,100.));
#30528=CARTESIAN_POINT('Ctrl Pts',(12.5267717721302,-12.2200650149237,0.134720657333168));
#30529=CARTESIAN_POINT('Ctrl Pts',(12.4986401261746,-12.2489027263458,0.163202546769506));
#30530=CARTESIAN_POINT('Ctrl Pts',(12.467152867614,-12.2742120695516,0.195519413317813));
#30531=CARTESIAN_POINT('Ctrl Pts',(12.3562405730693,-12.3432084553889,0.310543821638501));
#30532=CARTESIAN_POINT('Ctrl Pts',(12.2687615400859,-12.3688529339418,0.403057585612081));
#30533=CARTESIAN_POINT('Ctrl Pts',(12.1788144663232,-12.3708222676705,0.497903494267714));
#30534=CARTESIAN_POINT('Ctrl Pts',(12.1778203104535,-12.37084106725,0.498951748855235));
#30535=CARTESIAN_POINT('Ctrl Pts',(12.1768261106186,-12.3708569011015,0.5));
#30536=CARTESIAN_POINT('Origin',(12.2482946431511,-16.8583313034371,0.5));
#30537=CARTESIAN_POINT('Ctrl Pts',(3.12098026161582,-17.2452472912803,98.4746163542476));
#30538=CARTESIAN_POINT('Ctrl Pts',(2.89260432929213,-17.4018708609359,98.3611663178014));
#30539=CARTESIAN_POINT('Ctrl Pts',(2.75148341999934,-17.2923597286537,98.1210629636544));
#30540=CARTESIAN_POINT('Ctrl Pts',(2.73662446842811,-16.9531805857874,98.8304618827569));
#30541=CARTESIAN_POINT('Ctrl Pts',(2.54985248945744,-17.1146469822609,98.7002300650182));
#30542=CARTESIAN_POINT('Ctrl Pts',(2.41148044251108,-17.0285142699567,98.4769098403624));
#30543=CARTESIAN_POINT('Ctrl Pts',(2.2771369734248,-16.6926757665459,99.1602382875981));
#30544=CARTESIAN_POINT('Ctrl Pts',(2.1262371091352,-16.8482972498973,99.0255494138259));
#30545=CARTESIAN_POINT('Ctrl Pts',(2.00572321702946,-16.7928860538427,98.8066848982746));
#30546=CARTESIAN_POINT('Ctrl Pts',(1.48828850627735,-16.4115930339871,99.5229830380903));
#30547=CARTESIAN_POINT('Ctrl Pts',(1.3892948723609,-16.5617976914238,99.3820315078356));
#30548=CARTESIAN_POINT('Ctrl Pts',(1.31033409767429,-16.5384526486055,99.1694296468622));
#30549=CARTESIAN_POINT('Ctrl Pts',(1.20426376711607,-16.3348109530474,99.6234913693268));
#30550=CARTESIAN_POINT('Ctrl Pts',(1.12441622988636,-16.4834764139428,99.4807426095521));
#30551=CARTESIAN_POINT('Ctrl Pts',(1.06013194543906,-16.468911658045,99.2699379792856));
#30552=CARTESIAN_POINT('Ctrl Pts',(0.610116136352582,-16.2303876665528,
99.7608048122958));
#30553=CARTESIAN_POINT('Ctrl Pts',(0.570592580096315,-16.3774763782636,
99.6149071958598));
#30554=CARTESIAN_POINT('Ctrl Pts',(0.536982386432902,-16.3743182939754,
99.4072514211504));
#30555=CARTESIAN_POINT('Ctrl Pts',(0.304395385329841,-16.2034354627799,
99.7966027452517));
#30556=CARTESIAN_POINT('Ctrl Pts',(0.284158019240025,-16.3498801785155,
99.6501526042829));
#30557=CARTESIAN_POINT('Ctrl Pts',(0.267906895914237,-16.3498931438339,
99.4430493547679));
#30558=CARTESIAN_POINT('Ctrl Pts',(-0.155238398773932,-16.2036129415512,
99.79636776423));
#30559=CARTESIAN_POINT('Ctrl Pts',(-0.144919417032331,-16.350060507997,
99.6499229371967));
#30560=CARTESIAN_POINT('Ctrl Pts',(-0.136629658481305,-16.3500539600226,
99.442814373582));
#30561=CARTESIAN_POINT('Ctrl Pts',(-0.310467040971084,-16.2104925143924,
99.7872514480855));
#30562=CARTESIAN_POINT('Ctrl Pts',(-0.289967609306084,-16.3570649252483,
99.6409952531274));
#30563=CARTESIAN_POINT('Ctrl Pts',(-0.273250886059789,-16.3562879072327,
99.4336980572382));
#30564=CARTESIAN_POINT('Ctrl Pts',(-0.616270430045099,-16.2376016048274,
99.7514230350795));
#30565=CARTESIAN_POINT('Ctrl Pts',(-0.575332789987141,-16.3846026904707,
99.6059800049562));
#30566=CARTESIAN_POINT('Ctrl Pts',(-0.542427079965611,-16.3808502013102,
99.3978696447402));
#30567=CARTESIAN_POINT('Ctrl Pts',(-0.765900280742026,-16.2576126110768,
99.7250021223378));
#30568=CARTESIAN_POINT('Ctrl Pts',(-0.715021742305809,-16.4049628381993,
99.580115086457));
#30569=CARTESIAN_POINT('Ctrl Pts',(-0.674150359005859,-16.3989804855663,
99.3714487314956));
#30570=CARTESIAN_POINT('Ctrl Pts',(-1.20584020603565,-16.3354058480377,
99.6227146850676));
#30571=CARTESIAN_POINT('Ctrl Pts',(-1.12586029852611,-16.484076987348,99.4799874409064));
#30572=CARTESIAN_POINT('Ctrl Pts',(-1.06152132333177,-16.4694503946166,
99.2691612949723));
#30573=CARTESIAN_POINT('Ctrl Pts',(-1.49045845351357,-16.4122197672618,
99.5221656588586));
#30574=CARTESIAN_POINT('Ctrl Pts',(-1.39131820921651,-16.5624362368043,
99.3812294188917));
#30575=CARTESIAN_POINT('Ctrl Pts',(-1.31224595582822,-16.5390201922301,
99.1686122675856));
#30576=CARTESIAN_POINT('Ctrl Pts',(-2.01683567706171,-16.6000729369335,
99.2797533468154));
#30577=CARTESIAN_POINT('Ctrl Pts',(-1.87973999608329,-16.7526185023833,
99.1446071116388));
#30578=CARTESIAN_POINT('Ctrl Pts',(-1.77626230257574,-16.7090626239978,
98.9261999569019));
#30579=CARTESIAN_POINT('Ctrl Pts',(-2.26049125374327,-16.7108289072482,
99.1382521541653));
#30580=CARTESIAN_POINT('Ctrl Pts',(-2.10526006254958,-16.8650411275935,
99.0060308920462));
#30581=CARTESIAN_POINT('Ctrl Pts',(-1.99121820958417,-16.8092788783051,
98.7846987631132));
#30582=CARTESIAN_POINT('Ctrl Pts',(-2.71703050574155,-16.960436329805,98.8245648611909));
#30583=CARTESIAN_POINT('Ctrl Pts',(-2.52562525529546,-17.11676918777,98.7003130263028));
#30584=CARTESIAN_POINT('Ctrl Pts',(-2.39431788322546,-17.0350004816458,
98.4710114710564));
#30585=CARTESIAN_POINT('Ctrl Pts',(-2.92925959162701,-17.0995673036637,
98.6521093612485));
#30586=CARTESIAN_POINT('Ctrl Pts',(-2.71988721110581,-17.2571410628046,
98.5320184901546));
#30587=CARTESIAN_POINT('Ctrl Pts',(-2.58188146292343,-17.1607523397378,
98.2985618527006));
#30588=CARTESIAN_POINT('Ctrl Pts',(-3.12090206377705,-17.2451878710232,
98.4746887503082));
#30589=CARTESIAN_POINT('Ctrl Pts',(-2.89253316440024,-17.4018112264551,
98.3612367156073));
#30590=CARTESIAN_POINT('Ctrl Pts',(-2.75141424608767,-17.2923060501388,
98.1211353597149));
#30591=CARTESIAN_POINT('Ctrl Pts',(-2.57985201764259,-17.1655922764305,
98.2928932196501));
#30592=CARTESIAN_POINT('Ctrl Pts',(-2.60699083422014,-17.1846569627487,
98.3104738977108));
#30593=CARTESIAN_POINT('Ctrl Pts',(-2.63589822395985,-17.2009365925614,
98.3279440205353));
#30594=CARTESIAN_POINT('Ctrl Pts',(-2.66619302251831,-17.2142428928325,
98.3450378052742));
#30595=CARTESIAN_POINT('Ctrl Pts',(-2.69375391038932,-17.2263483851018,
98.3605889859024));
#30596=CARTESIAN_POINT('Ctrl Pts',(-2.72246604991279,-17.235993458018,98.3758286877673));
#30597=CARTESIAN_POINT('Ctrl Pts',(-2.75204644244987,-17.2429984586447,
98.3905567854016));
#30598=CARTESIAN_POINT('Ctrl Pts',(-2.77908636904687,-17.2494018457033,
98.4040199833104));
#30599=CARTESIAN_POINT('Ctrl Pts',(-2.80685349440489,-17.2535987038177,
98.4170556800783));
#30600=CARTESIAN_POINT('Ctrl Pts',(-2.83510492244771,-17.2554196617721,
98.4295110110486));
#30601=CARTESIAN_POINT('Ctrl Pts',(-2.86067249888962,-17.2570676309165,
98.4407831005944));
#30602=CARTESIAN_POINT('Ctrl Pts',(-2.88663747166555,-17.2567689298861,
98.4515798547762));
#30603=CARTESIAN_POINT('Ctrl Pts',(-2.91278154266259,-17.2543790789424,
98.4617879671636));
#30604=CARTESIAN_POINT('Ctrl Pts',(-2.9256874769523,-17.253199336918,98.4668271681246));
#30605=CARTESIAN_POINT('Ctrl Pts',(-2.93863637443791,-17.2515097647054,
98.4717229246966));
#30606=CARTESIAN_POINT('Ctrl Pts',(-2.95159725048241,-17.2492919759318,
98.4764616066469));
#30607=CARTESIAN_POINT('Ctrl Pts',(2.95159725048241,-17.2492919759318,98.4764616066469));
#30608=CARTESIAN_POINT('Ctrl Pts',(2.92468746478112,-17.2538966199715,98.4666230035037));
#30609=CARTESIAN_POINT('Ctrl Pts',(2.89776866146762,-17.256233666203,98.4560730110187));
#30610=CARTESIAN_POINT('Ctrl Pts',(2.87114106822738,-17.2564400451831,98.4449543865015));
#30611=CARTESIAN_POINT('Ctrl Pts',(2.84186545384406,-17.2566669478319,98.432730053611));
#30612=CARTESIAN_POINT('Ctrl Pts',(2.81294183068533,-17.254319064656,98.4198183682014));
#30613=CARTESIAN_POINT('Ctrl Pts',(2.78470495961941,-17.2495916469085,98.4064090535707));
#30614=CARTESIAN_POINT('Ctrl Pts',(2.75441171245854,-17.2445199506175,98.3920231932742));
#30615=CARTESIAN_POINT('Ctrl Pts',(2.72490814230923,-17.2367102069175,98.377064583912));
#30616=CARTESIAN_POINT('Ctrl Pts',(2.69654342034601,-17.2264059478322,98.3617674910395));
#30617=CARTESIAN_POINT('Ctrl Pts',(2.66333319619532,-17.2143414278847,98.3438572191246));
#30618=CARTESIAN_POINT('Ctrl Pts',(2.63168331085079,-17.1988577415842,98.3254829407057));
#30619=CARTESIAN_POINT('Ctrl Pts',(2.60208076598617,-17.1803381174911,98.3070206561472));
#30620=CARTESIAN_POINT('Ctrl Pts',(2.59453756232716,-17.1756190199655,98.3023161696555));
#30621=CARTESIAN_POINT('Ctrl Pts',(2.58712702122499,-17.1707027521616,98.2976059688177));
#30622=CARTESIAN_POINT('Ctrl Pts',(2.57985673374387,-17.1655955893933,98.2928962747544));
#30623=CARTESIAN_POINT('Origin',(-2.86726590046863,-16.7564550623337,100.));
#30624=CARTESIAN_POINT('Ctrl Pts',(-2.57985201635105,-17.1655922755232,
0.5));
#30625=CARTESIAN_POINT('Ctrl Pts',(-2.58066564781719,-17.1661638416687,
0.49895174885588));
#30626=CARTESIAN_POINT('Ctrl Pts',(-2.58148098692633,-17.166732982648,0.497903494266524));
#30627=CARTESIAN_POINT('Ctrl Pts',(-2.65540724343409,-17.2180093215811,
0.403057585761194));
#30628=CARTESIAN_POINT('Ctrl Pts',(-2.74125271403769,-17.2486813881429,
0.310543821736212));
#30629=CARTESIAN_POINT('Ctrl Pts',(-2.87153770337987,-17.2580547504885,
0.195519413315782));
#30630=CARTESIAN_POINT('Ctrl Pts',(-2.911887889342,-17.2560868079355,0.163202546768621));
#30631=CARTESIAN_POINT('Ctrl Pts',(-2.95159725048241,-17.2492919759318,
0.134720657333156));
#30632=CARTESIAN_POINT('Origin',(2.86726590046862,-16.7564550623337,100.));
#30633=CARTESIAN_POINT('Ctrl Pts',(2.95159725048241,-17.2492919759318,0.134720657333157));
#30634=CARTESIAN_POINT('Ctrl Pts',(2.91188788934223,-17.2560868079355,0.163202546768453));
#30635=CARTESIAN_POINT('Ctrl Pts',(2.8715377033803,-17.2580547504885,0.195519413315438));
#30636=CARTESIAN_POINT('Ctrl Pts',(2.74125271402536,-17.2486813881421,0.310543821747035));
#30637=CARTESIAN_POINT('Ctrl Pts',(2.65540724342468,-17.2180093215746,0.403057585777651));
#30638=CARTESIAN_POINT('Ctrl Pts',(2.58148098692613,-17.1667329826479,0.49790349426656));
#30639=CARTESIAN_POINT('Ctrl Pts',(2.58066564781731,-17.1661638416688,0.498951748855718));
#30640=CARTESIAN_POINT('Ctrl Pts',(2.57985201635104,-17.1655922755232,0.5));
#30641=CARTESIAN_POINT('Origin',(-2.55192432461455E-15,-20.8380434782609,
0.5));
#30642=CARTESIAN_POINT('Ctrl Pts',(-7.61153061250582,-15.7863147967496,
98.4745004885114));
#30643=CARTESIAN_POINT('Ctrl Pts',(-7.88836095469125,-15.7787835827682,
98.3610536502059));
#30644=CARTESIAN_POINT('Ctrl Pts',(-7.9381581147024,-15.6072288420487,98.1209470979181));
#30645=CARTESIAN_POINT('Ctrl Pts',(-7.68185024282998,-15.5529265513644,
98.6541872523937));
#30646=CARTESIAN_POINT('Ctrl Pts',(-7.94367437493447,-15.5575146677549,
98.5339912542897));
#30647=CARTESIAN_POINT('Ctrl Pts',(-7.99873405832647,-15.3985404288953,
98.3006281519147));
#30648=CARTESIAN_POINT('Ctrl Pts',(-7.77058558274001,-15.3193429185923,
98.8238114502904));
#30649=CARTESIAN_POINT('Ctrl Pts',(-8.01739572281288,-15.3332616605647,
98.6995854322395));
#30650=CARTESIAN_POINT('Ctrl Pts',(-8.07554514465372,-15.1898709314151,
98.4702580602194));
#30651=CARTESIAN_POINT('Ctrl Pts',(-7.9924298071297,-14.8502894771664,99.1368088098189));
#30652=CARTESIAN_POINT('Ctrl Pts',(-8.20881182371942,-14.883703165293,99.0046294469941));
#30653=CARTESIAN_POINT('Ctrl Pts',(-8.26829617652396,-14.7714171710724,
98.7832554187034));
#30654=CARTESIAN_POINT('Ctrl Pts',(-8.12737169382821,-14.6123994681448,
99.2813501417123));
#30655=CARTESIAN_POINT('Ctrl Pts',(-8.32776251015203,-14.6553398972789,
99.1461712456963));
#30656=CARTESIAN_POINT('Ctrl Pts',(-8.38583875689921,-14.5594769234819,
98.9277967516668));
#30657=CARTESIAN_POINT('Ctrl Pts',(-8.44228186665902,-14.1522925726334,
99.5228530262281));
#30658=CARTESIAN_POINT('Ctrl Pts',(-8.61067658867427,-14.2156092191235,
99.3819067332058));
#30659=CARTESIAN_POINT('Ctrl Pts',(-8.66083652547866,-14.1502985880832,
99.1692996350871));
#30660=CARTESIAN_POINT('Ctrl Pts',(-8.62238122769751,-13.9285751457649,
99.6211970158378));
#30661=CARTESIAN_POINT('Ctrl Pts',(-8.77477430608758,-14.0016497079299,
99.4784987699913));
#30662=CARTESIAN_POINT('Ctrl Pts',(-8.81839581871021,-13.9517156783976,
99.2676436259617));
#30663=CARTESIAN_POINT('Ctrl Pts',(-8.93504150578028,-13.6041086188705,
99.724700650501));
#30664=CARTESIAN_POINT('Ctrl Pts',(-9.06290937455646,-13.6933479875448,
99.5798189693958));
#30665=CARTESIAN_POINT('Ctrl Pts',(-9.09252380741154,-13.6644048462732,
99.3711472595492));
#30666=CARTESIAN_POINT('Ctrl Pts',(-9.04643201266491,-13.4980463524896,
99.7515464581424));
#30667=CARTESIAN_POINT('Ctrl Pts',(-9.1659008380529,-13.5929484631966,99.6061008493641));
#30668=CARTESIAN_POINT('Ctrl Pts',(-9.19027681092597,-13.5706128359882,
99.3979930676329));
#30669=CARTESIAN_POINT('Ctrl Pts',(-9.27641719553042,-13.297662320044,99.7871410858038));
#30670=CARTESIAN_POINT('Ctrl Pts',(-9.37920676320481,-13.404156206133,99.6408876188391));
#30671=CARTESIAN_POINT('Ctrl Pts',(-9.39230696146118,-13.3936667965263,
99.4335876951267));
#30672=CARTESIAN_POINT('Ctrl Pts',(-9.39592243526722,-13.2023470673547,
99.7962421951755));
#30673=CARTESIAN_POINT('Ctrl Pts',(-9.49053581390396,-13.3146274568229,
99.6498002056397));
#30674=CARTESIAN_POINT('Ctrl Pts',(-9.49738200583989,-13.3096324234838,
99.4426888046372));
#30675=CARTESIAN_POINT('Ctrl Pts',(-9.64409776558335,-13.0216618073135,
99.7966442229661));
#30676=CARTESIAN_POINT('Ctrl Pts',(-9.72219875439405,-13.1459331194972,
99.6501931431456));
#30677=CARTESIAN_POINT('Ctrl Pts',(-9.71580342119468,-13.1505998825526,
99.4430908323178));
#30678=CARTESIAN_POINT('Ctrl Pts',(-9.77381197449095,-12.9356824620425,
99.7877849805069));
#30679=CARTESIAN_POINT('Ctrl Pts',(-9.84373626500581,-13.0660445920766,
99.6415170968033));
#30680=CARTESIAN_POINT('Ctrl Pts',(-9.83007072703063,-13.0750678730396,
99.4342315896588));
#30681=CARTESIAN_POINT('Ctrl Pts',(-10.0376062905057,-12.7771593103382,
99.7523547967177));
#30682=CARTESIAN_POINT('Ctrl Pts',(-10.0912047848049,-12.9199070101996,
99.6068909575268));
#30683=CARTESIAN_POINT('Ctrl Pts',(-10.0626757487172,-12.9360922565949,
99.3988014063792));
#30684=CARTESIAN_POINT('Ctrl Pts',(-10.1706575690792,-12.7050827268415,
99.7260859669308));
#30685=CARTESIAN_POINT('Ctrl Pts',(-10.2163999615544,-12.8539677361418,
99.581174605591));
#30686=CARTESIAN_POINT('Ctrl Pts',(-10.1801044201994,-12.8730550738084,
99.3725325760877));
#30687=CARTESIAN_POINT('Ctrl Pts',(-10.5730247519993,-12.5085765171443,
99.6241384720944));
#30688=CARTESIAN_POINT('Ctrl Pts',(-10.5959433339685,-12.6756716426713,
99.4813799591445));
#30689=CARTESIAN_POINT('Ctrl Pts',(-10.5355461919898,-12.7016211074057,
99.2705850820007));
#30690=CARTESIAN_POINT('Ctrl Pts',(-10.8489658974378,-12.4029669023366,
99.5236562902266));
#30691=CARTESIAN_POINT('Ctrl Pts',(-10.8572640774209,-12.5825975767434,
99.3826839740364));
#30692=CARTESIAN_POINT('Ctrl Pts',(-10.7797437745015,-12.6101276716056,
99.1701028989501));
#30693=CARTESIAN_POINT('Ctrl Pts',(-11.3863904046298,-12.2448379356151,
99.2810827044785));
#30694=CARTESIAN_POINT('Ctrl Pts',(-11.3652836467698,-12.4487162064104,
99.1459030339944));
#30695=CARTESIAN_POINT('Ctrl Pts',(-11.2561108367434,-12.474332324694,98.9275293145685));
#30696=CARTESIAN_POINT('Ctrl Pts',(-11.6491602608148,-12.1909944678519,
99.1393951997109));
#30697=CARTESIAN_POINT('Ctrl Pts',(-11.6143348897636,-12.4069069268349,
99.0071411174915));
#30698=CARTESIAN_POINT('Ctrl Pts',(-11.489403766598,-12.4288617015343,98.7858418086588));
#30699=CARTESIAN_POINT('Ctrl Pts',(-12.1662817650126,-12.1242950353399,
98.8252029000679));
#30700=CARTESIAN_POINT('Ctrl Pts',(-12.1033811314411,-12.3632333592681,
98.7009299069291));
#30701=CARTESIAN_POINT('Ctrl Pts',(-11.9491322142495,-12.3742909202748,
98.4716495099335));
#30702=CARTESIAN_POINT('Ctrl Pts',(-12.4202878510302,-12.1120529425579,
98.6524117207795));
#30703=CARTESIAN_POINT('Ctrl Pts',(-12.3435537205759,-12.362581638257,98.5323055644746));
#30704=CARTESIAN_POINT('Ctrl Pts',(-12.1752607824295,-12.365734055554,98.2988642625954));
#30705=CARTESIAN_POINT('Ctrl Pts',(-12.6613982812294,-12.1172313198433,
98.4746383405503));
#30706=CARTESIAN_POINT('Ctrl Pts',(-12.5687009849841,-12.378177146358,98.3611876972422));
#30707=CARTESIAN_POINT('Ctrl Pts',(-12.3901642949233,-12.3725306764959,
98.121084949957));
#30708=CARTESIAN_POINT('Ctrl Pts',(-12.1768261122223,-12.3708569010759,
98.2928932196637));
#30709=CARTESIAN_POINT('Ctrl Pts',(-12.2099878174022,-12.3703287601507,
98.310473897661));
#30710=CARTESIAN_POINT('Ctrl Pts',(-12.2429433131837,-12.366507919979,98.3279440204279));
#30711=CARTESIAN_POINT('Ctrl Pts',(-12.2752735670263,-12.3594661072555,
98.3450378051151));
#30712=CARTESIAN_POINT('Ctrl Pts',(-12.304686223498,-12.3530597728176,98.3605889857293));
#30713=CARTESIAN_POINT('Ctrl Pts',(-12.3335840639116,-12.3439862285719,
98.3758286875838));
#30714=CARTESIAN_POINT('Ctrl Pts',(-12.3616325402144,-12.3322664746665,
98.3905567852105));
#30715=CARTESIAN_POINT('Ctrl Pts',(-12.3872721168296,-12.3215532535657,
98.4040199831191));
#30716=CARTESIAN_POINT('Ctrl Pts',(-12.4122030444301,-12.3086274763456,
98.4170556798887));
#30717=CARTESIAN_POINT('Ctrl Pts',(-12.4361292620607,-12.2934948895455,
98.4295110108618));
#30718=CARTESIAN_POINT('Ctrl Pts',(-12.4577825178641,-12.2797998802462,
98.4407831004098));
#30719=CARTESIAN_POINT('Ctrl Pts',(-12.4786130500376,-12.2642963979904,
98.4515798545948));
#30720=CARTESIAN_POINT('Ctrl Pts',(-12.4983593286395,-12.2469958686251,
98.4617879669855));
#30721=CARTESIAN_POINT('Ctrl Pts',(-12.5081070139649,-12.2384555193463,
98.4668271680095));
#30722=CARTESIAN_POINT('Ctrl Pts',(-12.5175897865744,-12.2294774556375,
98.471722924641));
#30723=CARTESIAN_POINT('Ctrl Pts',(-12.5267717721302,-12.2200650149237,
98.4764616066469));
#30724=CARTESIAN_POINT('Origin',(-7.5273854258457,-15.2389652386414,98.2808710159383));
#30725=CARTESIAN_POINT('Origin',(-12.1688640072122,-11.8709203002116,100.));
#30726=CARTESIAN_POINT('Ctrl Pts',(-12.1768261106186,-12.3708569011015,
0.5));
#30727=CARTESIAN_POINT('Ctrl Pts',(-12.1778203104535,-12.37084106725,0.498951748855216));
#30728=CARTESIAN_POINT('Ctrl Pts',(-12.1788144663228,-12.3708222676705,
0.497903494267674));
#30729=CARTESIAN_POINT('Ctrl Pts',(-12.2687615400609,-12.3688529339424,
0.403057585648595));
#30730=CARTESIAN_POINT('Ctrl Pts',(-12.3562405730462,-12.3432084554035,
0.31054382166245));
#30731=CARTESIAN_POINT('Ctrl Pts',(-12.4671528676144,-12.2742120695513,
0.19551941331738));
#30732=CARTESIAN_POINT('Ctrl Pts',(-12.4986401261748,-12.2489027263456,
0.163202546769333));
#30733=CARTESIAN_POINT('Ctrl Pts',(-12.5267717721302,-12.2200650149237,
0.134720657333167));
#30734=CARTESIAN_POINT('Origin',(-7.52953032547043,-15.2415935216047,100.));
#30735=CARTESIAN_POINT('Ctrl Pts',(-7.75098709974897,-15.6898756840048,
0.134720657333167));
#30736=CARTESIAN_POINT('Ctrl Pts',(-7.7871065497921,-15.6720322417129,0.163202546769531));
#30737=CARTESIAN_POINT('Ctrl Pts',(-7.82090726357263,-15.6499070964456,
0.195519413317832));
#30738=CARTESIAN_POINT('Ctrl Pts',(-7.92080050981464,-15.5657442917632,
0.310543821628375));
#30739=CARTESIAN_POINT('Ctrl Pts',(-7.97222236609799,-15.4904713670923,
0.403057585596688));
#30740=CARTESIAN_POINT('Ctrl Pts',(-8.00189048816371,-15.405535174049,0.497903494267389));
#30741=CARTESIAN_POINT('Ctrl Pts',(-8.00221557868521,-15.4045954850201,
0.498951748855124));
#30742=CARTESIAN_POINT('Ctrl Pts',(-8.00253786221767,-15.4036548377177,
0.5));
#30743=CARTESIAN_POINT('Origin',(-12.2482946431511,-16.8583313034371,0.5));
#30744=CARTESIAN_POINT('Ctrl Pts',(-17.3143275672679,-2.71461308511347,
98.1029310402112));
#30745=CARTESIAN_POINT('Ctrl Pts',(-17.4636977395246,-2.61423858422028,
98.3435819248339));
#30746=CARTESIAN_POINT('Ctrl Pts',(-17.3857742401592,-2.34690286062856,
98.456536910202));
#30747=CARTESIAN_POINT('Ctrl Pts',(-17.1296512857755,-2.83873298507897,
98.2878840680197));
#30748=CARTESIAN_POINT('Ctrl Pts',(-17.2651608222781,-2.73703317200584,
98.5214982033383));
#30749=CARTESIAN_POINT('Ctrl Pts',(-17.1800764225947,-2.48819271345443,
98.6414834344728));
#30750=CARTESIAN_POINT('Ctrl Pts',(-16.9451136614061,-2.98310069421631,
98.4673409000723));
#30751=CARTESIAN_POINT('Ctrl Pts',(-17.0639661471992,-2.88326764442847,
98.6966806273241));
#30752=CARTESIAN_POINT('Ctrl Pts',(-16.9743943558017,-2.65255720277051,
98.8209468545885));
#30753=CARTESIAN_POINT('Ctrl Pts',(-16.599710139157,-3.30279942760483,98.7866059478771));
#30754=CARTESIAN_POINT('Ctrl Pts',(-16.6878268341941,-3.21163443205236,
99.0079277681159));
#30755=CARTESIAN_POINT('Ctrl Pts',(-16.5890378089614,-3.01654651232763,
99.1402125820154));
#30756=CARTESIAN_POINT('Ctrl Pts',(-16.4374762686563,-3.47698561123553,
98.9284804941285));
#30757=CARTESIAN_POINT('Ctrl Pts',(-16.5106768516081,-3.39212226297961,
99.1468659074355));
#30758=CARTESIAN_POINT('Ctrl Pts',(-16.4078485131273,-3.21487371577898,
99.282087448839));
#30759=CARTESIAN_POINT('Ctrl Pts',(-16.2075579278768,-3.77068327953477,
99.1108598027294));
#30760=CARTESIAN_POINT('Ctrl Pts',(-16.2598042688104,-3.699711420573,99.3254864613232));
#30761=CARTESIAN_POINT('Ctrl Pts',(-16.1506324221157,-3.54922452427082,
99.4644671720467));
#30762=CARTESIAN_POINT('Ctrl Pts',(-16.1328338869384,-3.87465067488062,
99.1667281040793));
#30763=CARTESIAN_POINT('Ctrl Pts',(-16.1785346664591,-3.80861210815923,
99.3801095631261));
#30764=CARTESIAN_POINT('Ctrl Pts',(-16.066957542548,-3.66757422893071,99.5203355960163));
#30765=CARTESIAN_POINT('Ctrl Pts',(-15.9919866048145,-4.0899475674556,99.2638527346786));
#30766=CARTESIAN_POINT('Ctrl Pts',(-16.0257056636234,-4.03466861210512,
99.4749661095219));
#30767=CARTESIAN_POINT('Ctrl Pts',(-15.9090517391358,-3.91261572849114,
99.6174604374821));
#30768=CARTESIAN_POINT('Ctrl Pts',(-15.9254898327248,-4.20166713029529,
99.30543993253));
#30769=CARTESIAN_POINT('Ctrl Pts',(-15.9535873993429,-4.15233969324173,
99.515658214164));
#30770=CARTESIAN_POINT('Ctrl Pts',(-15.834403694553,-4.03975173211336,99.6590477275195));
#30771=CARTESIAN_POINT('Ctrl Pts',(-15.738603988475,-4.55006349017939,99.407174605891));
#30772=CARTESIAN_POINT('Ctrl Pts',(-15.7519852189442,-4.51914563857056,
99.6148745113244));
#30773=CARTESIAN_POINT('Ctrl Pts',(-15.6242698911513,-4.43612723332494,
99.7607826165559));
#30774=CARTESIAN_POINT('Ctrl Pts',(-15.6300705661688,-4.80379339451677,
99.4435386777497));
#30775=CARTESIAN_POINT('Ctrl Pts',(-15.6349263242121,-4.78871307695036,
99.6506668510312));
#30776=CARTESIAN_POINT('Ctrl Pts',(-15.501725341209,-4.72466850699754,99.7971467765044));
#30777=CARTESIAN_POINT('Ctrl Pts',(-15.5059824861585,-5.18799157661508,
99.4425027003972));
#30778=CARTESIAN_POINT('Ctrl Pts',(-15.5033523953773,-5.19622875259016,
99.6496543232893));
#30779=CARTESIAN_POINT('Ctrl Pts',(-15.3607119866153,-5.1611950812275,99.7961107967627));
#30780=CARTESIAN_POINT('Ctrl Pts',(-15.4705223787628,-5.31743764272474,
99.4333242900206));
#30781=CARTESIAN_POINT('Ctrl Pts',(-15.466074874266,-5.33377871102699,99.6406660872409));
#30782=CARTESIAN_POINT('Ctrl Pts',(-15.3202268375058,-5.30821065016262,
99.786932365797));
#30783=CARTESIAN_POINT('Ctrl Pts',(-15.4112870235324,-5.57906517882993,
99.3975703058089));
#30784=CARTESIAN_POINT('Ctrl Pts',(-15.4046994857703,-5.61160402086348,
99.605723827768));
#30785=CARTESIAN_POINT('Ctrl Pts',(-15.2521751775211,-5.60519824976417,
99.7511783033391));
#30786=CARTESIAN_POINT('Ctrl Pts',(-15.3873774999491,-5.71249818528166,
99.370619399419));
#30787=CARTESIAN_POINT('Ctrl Pts',(-15.3804432938941,-5.75346933726169,
99.5793392014518));
#30788=CARTESIAN_POINT('Ctrl Pts',(-15.2244484235508,-5.75658897920125,
99.7242273368566));
#30789=CARTESIAN_POINT('Ctrl Pts',(-15.3346696945248,-6.10616299653759,
99.2668124456042));
#30790=CARTESIAN_POINT('Ctrl Pts',(-15.3287678592426,-6.17236078267475,
99.4777222783444));
#30791=CARTESIAN_POINT('Ctrl Pts',(-15.1624256089298,-6.20298061454582,
99.6204201490477));
#30792=CARTESIAN_POINT('Ctrl Pts',(-15.3240667024475,-6.35937968875464,
99.1683014346688));
#30793=CARTESIAN_POINT('Ctrl Pts',(-15.3219320743537,-6.44185472978044,
99.3809681438969));
#30794=CARTESIAN_POINT('Ctrl Pts',(-15.1483769580277,-6.48977650021881,
99.5219089068377));
#30795=CARTESIAN_POINT('Ctrl Pts',(-15.3423230787144,-6.8517981468712,98.9266153300885));
#30796=CARTESIAN_POINT('Ctrl Pts',(-15.3517693972098,-6.9636263391151,99.1450562468822));
#30797=CARTESIAN_POINT('Ctrl Pts',(-15.1643067184423,-7.04682949241124,
99.2802222813138));
#30798=CARTESIAN_POINT('Ctrl Pts',(-15.3719403060825,-7.09247220631558,
98.7818489409676));
#30799=CARTESIAN_POINT('Ctrl Pts',(-15.389921523533,-7.21841417521539,99.0032991843689));
#30800=CARTESIAN_POINT('Ctrl Pts',(-15.1951156833261,-7.31874252774749,
99.1354555654038));
#30801=CARTESIAN_POINT('Ctrl Pts',(-15.4635565835937,-7.55131386467538,
98.463752920865));
#30802=CARTESIAN_POINT('Ctrl Pts',(-15.5012645827008,-7.70215187775885,
98.693197017485));
#30803=CARTESIAN_POINT('Ctrl Pts',(-15.2930580254491,-7.83652577451189,
98.8173588681435));
#30804=CARTESIAN_POINT('Ctrl Pts',(-15.5265390080494,-7.77132456514675,
98.288422358841));
#30805=CARTESIAN_POINT('Ctrl Pts',(-15.5763509022929,-7.93321211455735,
98.5220290044167));
#30806=CARTESIAN_POINT('Ctrl Pts',(-15.3612680514613,-8.08445864282625,
98.6420342840825));
#30807=CARTESIAN_POINT('Ctrl Pts',(-15.603214142857,-7.98099597085232,98.102881938306));
#30808=CARTESIAN_POINT('Ctrl Pts',(-15.6650624954312,-8.15000252613851,
98.3435328810485));
#30809=CARTESIAN_POINT('Ctrl Pts',(-15.4448833406397,-8.32048399586279,
98.4564865389123));
#30810=CARTESIAN_POINT('Ctrl Pts',(-17.1226665060507,-2.85087466017704,
98.292893219028));
#30811=CARTESIAN_POINT('Ctrl Pts',(-17.1491844558325,-2.83095542391483,
98.310473897128));
#30812=CARTESIAN_POINT('Ctrl Pts',(-17.1736001786359,-2.80849354481796,
98.3279440199927));
#30813=CARTESIAN_POINT('Ctrl Pts',(-17.1956168299013,-2.78379335215336,
98.3450378047718));
#30814=CARTESIAN_POINT('Ctrl Pts',(-17.2156466200124,-2.7613221929924,98.3605889854306));
#30815=CARTESIAN_POINT('Ctrl Pts',(-17.2336921685873,-2.73699581704382,
98.3758286873264));
#30816=CARTESIAN_POINT('Ctrl Pts',(-17.2494951641405,-2.71102785619787,
98.3905567849915));
#30817=CARTESIAN_POINT('Ctrl Pts',(-17.2639409440285,-2.68729011323276,
98.4040199829228));
#30818=CARTESIAN_POINT('Ctrl Pts',(-17.2765129069594,-2.66217890820016,
98.4170556797135));
#30819=CARTESIAN_POINT('Ctrl Pts',(-17.2869749123189,-2.63587291041262,
98.429511010707));
#30820=CARTESIAN_POINT('Ctrl Pts',(-17.2964430397793,-2.61206595070767,
98.4407831002688));
#30821=CARTESIAN_POINT('Ctrl Pts',(-17.3041825761053,-2.58727949046054,
98.4515798544673));
#30822=CARTESIAN_POINT('Ctrl Pts',(-17.3099886550732,-2.56167649681956,
98.461787966872));
#30823=CARTESIAN_POINT('Ctrl Pts',(-17.3128548068309,-2.54903766334346,
98.4668271679356));
#30824=CARTESIAN_POINT('Ctrl Pts',(-17.3152493576056,-2.53620042323942,
98.471722924605));
#30825=CARTESIAN_POINT('Ctrl Pts',(-17.3171452461371,-2.52318856294818,
98.4764616066469));
#30826=CARTESIAN_POINT('Origin',(-15.0469618583258,-7.90408080222984,98.2808650734415));
#30827=CARTESIAN_POINT('Origin',(-16.822369667676,-2.45109746114966,100.));
#30828=CARTESIAN_POINT('Ctrl Pts',(-17.122666505727,-2.85087466042014,0.5));
#30829=CARTESIAN_POINT('Ctrl Pts',(-17.1234615233844,-2.85027747456476,
0.498951748855855));
#30830=CARTESIAN_POINT('Ctrl Pts',(-17.1242547622617,-2.84967791522736,
0.497903494266366));
#30831=CARTESIAN_POINT('Ctrl Pts',(-17.1958659280832,-2.79521512742361,
0.403057585843291));
#30832=CARTESIAN_POINT('Ctrl Pts',(-17.2515645061835,-2.72304942305474,
0.310543821790061));
#30833=CARTESIAN_POINT('Ctrl Pts',(-17.3007393793638,-2.60203756316618,
0.195519413314588));
#30834=CARTESIAN_POINT('Ctrl Pts',(-17.3113366479633,-2.56305412818102,
0.163202546768072));
#30835=CARTESIAN_POINT('Ctrl Pts',(-17.3171452461371,-2.52318856294818,
0.134720657333154));
#30836=CARTESIAN_POINT('Origin',(-15.0503018864028,-7.90496129833282,100.));
#30837=CARTESIAN_POINT('Ctrl Pts',(-15.4929578242382,-8.13746016004849,
0.134720657333154));
#30838=CARTESIAN_POINT('Ctrl Pts',(-15.5116909609204,-8.10179403194155,
0.163202546768232));
#30839=CARTESIAN_POINT('Ctrl Pts',(-15.5260314786975,-8.06402685234187,
0.195519413314936));
#30840=CARTESIAN_POINT('Ctrl Pts',(-15.5573771571874,-7.93722193595586,
0.310543821769176));
#30841=CARTESIAN_POINT('Ctrl Pts',(-15.5547339977031,-7.84609985192745,
0.403057585811652));
#30842=CARTESIAN_POINT('Ctrl Pts',(-15.5288117710302,-7.7599465438431,0.497903494266294));
#30843=CARTESIAN_POINT('Ctrl Pts',(-15.5285224394342,-7.75899523603616,
0.498951748855642));
#30844=CARTESIAN_POINT('Ctrl Pts',(-15.5282302736771,-7.75804480287585,
0.5));
#30845=CARTESIAN_POINT('Origin',(-19.8181570368417,-6.43930956430665,0.5));
#30846=CARTESIAN_POINT('Ctrl Pts',(-17.3656407514415,2.36084587016586,98.4746163542476));
#30847=CARTESIAN_POINT('Ctrl Pts',(-17.4440265737737,2.62644363351055,98.3611663178014));
#30848=CARTESIAN_POINT('Ctrl Pts',(-17.2962665385767,2.72681679293049,98.1210629636544));
#30849=CARTESIAN_POINT('Ctrl Pts',(-16.9690963360076,2.6361363763642,98.8304618827575));
#30850=CARTESIAN_POINT('Ctrl Pts',(-17.0649442889615,2.86366294455722,98.7002300650182));
#30851=CARTESIAN_POINT('Ctrl Pts',(-16.940267897606,2.96864610960449,98.4769098403635));
#30852=CARTESIAN_POINT('Ctrl Pts',(-16.5793520854839,2.99263453638016,99.160238287598));
#30853=CARTESIAN_POINT('Ctrl Pts',(-16.6807262887868,3.18423851866632,99.0255494138259));
#30854=CARTESIAN_POINT('Ctrl Pts',(-16.5907862689845,3.2817310397979,98.8066848982746));
#30855=CARTESIAN_POINT('Ctrl Pts',(-16.06825893873,3.65601467024584,99.5229830380904));
#30856=CARTESIAN_POINT('Ctrl Pts',(-16.1805213417477,3.7965790026359,99.3820315078356));
#30857=CARTESIAN_POINT('Ctrl Pts',(-16.133918665385,3.86446114696819,99.1694296468622));
#30858=CARTESIAN_POINT('Ctrl Pts',(-15.9074663690937,3.90241128133996,99.6234913693271));
#30859=CARTESIAN_POINT('Ctrl Pts',(-16.0241813784637,4.02429095582591,99.480742609552));
#30860=CARTESIAN_POINT('Ctrl Pts',(-15.9904645360932,4.08092818635339,99.2699379792856));
#30861=CARTESIAN_POINT('Ctrl Pts',(-15.6245522069473,4.43521068708326,99.7608048122955));
#30862=CARTESIAN_POINT('Ctrl Pts',(-15.7522284341316,4.51825273440706,99.6149071958598));
#30863=CARTESIAN_POINT('Ctrl Pts',(-15.7388387964642,4.54924202638999,99.4072514211504));
#30864=CARTESIAN_POINT('Ctrl Pts',(-15.504446230321,4.71763971050837,99.7966027452519));
#30865=CARTESIAN_POINT('Ctrl Pts',(-15.637469741455,4.7821404952994,99.6501526042829));
#30866=CARTESIAN_POINT('Ctrl Pts',(-15.6324601989205,4.79760023853937,99.4430493547679));
#30867=CARTESIAN_POINT('Ctrl Pts',(-15.3625803721861,5.15483225994642,99.79636776423));
#30868=CARTESIAN_POINT('Ctrl Pts',(-15.5050490252728,5.19027311193616,99.6499229371967));
#30869=CARTESIAN_POINT('Ctrl Pts',(-15.5076044740504,5.18238705961226,99.442814373582));
#30870=CARTESIAN_POINT('Ctrl Pts',(-15.3211549463132,5.30458937654559,99.7872514480856));
#30871=CARTESIAN_POINT('Ctrl Pts',(-15.4668882655262,5.33038662434119,99.6409952531274));
#30872=CARTESIAN_POINT('Ctrl Pts',(-15.4713150290528,5.31424796399505,99.4336980572382));
#30873=CARTESIAN_POINT('Ctrl Pts',(-15.2524387792612,5.60380285207595,99.7514230350794));
#30874=CARTESIAN_POINT('Ctrl Pts',(-15.4048955461524,5.61029467639245,99.6059800049562));
#30875=CARTESIAN_POINT('Ctrl Pts',(-15.4114951404923,5.57783990353127,99.3978696447402));
#30876=CARTESIAN_POINT('Ctrl Pts',(-15.2252322104212,5.75229303761896,99.7250021223377));
#30877=CARTESIAN_POINT('Ctrl Pts',(-15.3810929371293,5.74943839640557,99.580115086457));
#30878=CARTESIAN_POINT('Ctrl Pts',(-15.3880333336981,5.70871875235814,99.3714487314956));
#30879=CARTESIAN_POINT('Ctrl Pts',(-15.1632690619361,6.19474020261685,99.6227146850678));
#30880=CARTESIAN_POINT('Ctrl Pts',(-15.3293788683914,6.16461669902704,99.4799874409064));
#30881=CARTESIAN_POINT('Ctrl Pts',(-15.3353499887989,6.09890683169306,99.2691612949723));
#30882=CARTESIAN_POINT('Ctrl Pts',(-15.148371564977,6.48916504798086,99.5221656588589));
#30883=CARTESIAN_POINT('Ctrl Pts',(-15.3218719375044,6.44129651453844,99.3812294188918));
#30884=CARTESIAN_POINT('Ctrl Pts',(-15.3240366258068,6.35885837698121,99.1686122675856));
#30885=CARTESIAN_POINT('Ctrl Pts',(-15.1643710385716,7.04782935834292,99.2797533468151));
#30886=CARTESIAN_POINT('Ctrl Pts',(-15.3518153879025,6.96458278973326,99.1446071116388));
#30887=CARTESIAN_POINT('Ctrl Pts',(-15.3423676517735,6.85271014840536,98.9261999569019));
#30888=CARTESIAN_POINT('Ctrl Pts',(-15.1944125118882,7.3137850593314,99.1382521541667));
#30889=CARTESIAN_POINT('Ctrl Pts',(-15.3890461250777,7.21380562024102,99.0060308920463));
#30890=CARTESIAN_POINT('Ctrl Pts',(-15.3712539451641,7.08811389017403,98.7846987631153));
#30891=CARTESIAN_POINT('Ctrl Pts',(-15.2907248901618,7.82511262538337,98.8245648611895));
#30892=CARTESIAN_POINT('Ctrl Pts',(-15.4985537486391,7.69138492458409,98.7003130263029));
#30893=CARTESIAN_POINT('Ctrl Pts',(-15.461363297308,7.54123627293827,98.4710114710543));
#30894=CARTESIAN_POINT('Ctrl Pts',(-15.3574639152262,8.06994831582745,98.6521093612504));
#30895=CARTESIAN_POINT('Ctrl Pts',(-15.5720250893883,7.91951631844514,98.5320184901583));
#30896=CARTESIAN_POINT('Ctrl Pts',(-15.5230000877306,7.75847929885542,98.298561852705));
#30897=CARTESIAN_POINT('Ctrl Pts',(-15.4367365239838,8.29721036780905,98.4746887503082));
#30898=CARTESIAN_POINT('Ctrl Pts',(-15.6562640576654,8.12841791648205,98.3612367156073));
#30899=CARTESIAN_POINT('Ctrl Pts',(-15.5957265901482,7.96036688919461,98.1211353597149));
#30900=CARTESIAN_POINT('Ctrl Pts',(-15.5282302741409,7.75804480438455,98.2928932196501));
#30901=CARTESIAN_POINT('Ctrl Pts',(-15.5379755127708,7.78974666481774,98.3104738977231));
#30902=CARTESIAN_POINT('Ctrl Pts',(-15.5445254860964,7.82226990849227,98.3279440205588));
#30903=CARTESIAN_POINT('Ctrl Pts',(-15.5478189220795,7.85519384700696,98.3450378053077));
#30904=CARTESIAN_POINT('Ctrl Pts',(-15.5508151466501,7.88514661185367,98.3605889859386));
#30905=CARTESIAN_POINT('Ctrl Pts',(-15.5511156170357,7.91543397069313,98.3758286878054));
#30906=CARTESIAN_POINT('Ctrl Pts',(-15.5486369245292,7.94573126001502,98.390556785441));
#30907=CARTESIAN_POINT('Ctrl Pts',(-15.5463711106682,7.97342651383039,98.4040199833497));
#30908=CARTESIAN_POINT('Ctrl Pts',(-15.5417820463004,8.00113151982359,98.4170556801172));
#30909=CARTESIAN_POINT('Ctrl Pts',(-15.5347837088429,8.0285629315143,98.4295110110869));
#30910=CARTESIAN_POINT('Ctrl Pts',(-15.5284502050059,8.05338839216903,98.4407831006321));
#30911=CARTESIAN_POINT('Ctrl Pts',(-15.5201425055928,8.07799024503,98.4515798548133));
#30912=CARTESIAN_POINT('Ctrl Pts',(-15.5097906600338,8.10211622955971,98.4617879672));
#30913=CARTESIAN_POINT('Ctrl Pts',(-15.5046805056801,8.1140259421013,98.4668271681481));
#30914=CARTESIAN_POINT('Ctrl Pts',(-15.4990721976482,8.12581896887833,98.4717229247079));
#30915=CARTESIAN_POINT('Ctrl Pts',(-15.4929578242382,8.13746016004849,98.4764616066469));
#30916=CARTESIAN_POINT('Ctrl Pts',(-17.3171452461371,2.52318856294819,98.4764616066469));
#30917=CARTESIAN_POINT('Ctrl Pts',(-17.3132089417596,2.55020420325263,98.4666230035038));
#30918=CARTESIAN_POINT('Ctrl Pts',(-17.3071132371149,2.57652769355676,98.4560730110189));
#30919=CARTESIAN_POINT('Ctrl Pts',(-17.2990811363583,2.60191581423307,98.4449543865016));
#30920=CARTESIAN_POINT('Ctrl Pts',(-17.2902502712358,2.62982869483543,98.4327300536111));
#30921=CARTESIAN_POINT('Ctrl Pts',(-17.279079410547,2.65661115931325,98.4198183682014));
#30922=CARTESIAN_POINT('Ctrl Pts',(-17.2658576960657,2.6820051671168,98.4064090535706));
#30923=CARTESIAN_POINT('Ctrl Pts',(-17.2516730980718,2.70924851688491,98.3920231932739));
#30924=CARTESIAN_POINT('Ctrl Pts',(-17.2351284858644,2.73489473600463,98.3770645839114));
#30925=CARTESIAN_POINT('Ctrl Pts',(-17.2165633719882,2.75868699848906,98.3617674910388));
#30926=CARTESIAN_POINT('Ctrl Pts',(-17.1948268080254,2.78654365688397,98.343857219123));
#30927=CARTESIAN_POINT('Ctrl Pts',(-17.17032059483,2.81185976437969,98.3254829407031));
#30928=CARTESIAN_POINT('Ctrl Pts',(-17.1435596962152,2.83429057899883,98.3070206561438));
#30929=CARTESIAN_POINT('Ctrl Pts',(-17.1367405896413,2.84000631065752,98.3023161696533));
#30930=CARTESIAN_POINT('Ctrl Pts',(-17.1297749579741,2.84553494376039,98.2976059688167));
#30931=CARTESIAN_POINT('Ctrl Pts',(-17.1226711151596,2.85087119795497,98.2928962747546));
#30932=CARTESIAN_POINT('Origin',(-15.0503018864028,7.90496129833282,100.));
#30933=CARTESIAN_POINT('Ctrl Pts',(-15.5282302736771,7.75804480287585,0.5));
#30934=CARTESIAN_POINT('Ctrl Pts',(-15.5285224394341,7.75899523603604,0.498951748855783));
#30935=CARTESIAN_POINT('Ctrl Pts',(-15.5288117710301,7.75994654384298,0.497903494266496));
#30936=CARTESIAN_POINT('Ctrl Pts',(-15.5547339977038,7.84609985192962,0.403057585807818));
#30937=CARTESIAN_POINT('Ctrl Pts',(-15.5573771571867,7.93722193595853,0.310543821766792));
#30938=CARTESIAN_POINT('Ctrl Pts',(-15.5260314786975,8.06402685234172,0.195519413315069));
#30939=CARTESIAN_POINT('Ctrl Pts',(-15.5116909609204,8.10179403194149,0.163202546768283));
#30940=CARTESIAN_POINT('Ctrl Pts',(-15.4929578242382,8.13746016004849,0.134720657333155));
#30941=CARTESIAN_POINT('Origin',(-16.822369667676,2.45109746114966,100.));
#30942=CARTESIAN_POINT('Ctrl Pts',(-17.3171452461371,2.52318856294819,0.134720657333156));
#30943=CARTESIAN_POINT('Ctrl Pts',(-17.3113366479633,2.56305412818148,0.163202546768402));
#30944=CARTESIAN_POINT('Ctrl Pts',(-17.3007393793636,2.60203756316703,0.195519413315302));
#30945=CARTESIAN_POINT('Ctrl Pts',(-17.2515645061962,2.72304942302292,0.310543821760042));
#30946=CARTESIAN_POINT('Ctrl Pts',(-17.1958659281084,2.79521512740442,0.403057585797637));
#30947=CARTESIAN_POINT('Ctrl Pts',(-17.124254762262,2.84967791522717,0.497903494266591));
#30948=CARTESIAN_POINT('Ctrl Pts',(-17.1234615233845,2.85027747456468,0.498951748855702));
#30949=CARTESIAN_POINT('Ctrl Pts',(-17.122666505727,2.85087466042014,0.5));
#30950=CARTESIAN_POINT('Origin',(-19.8181570368417,6.43930956430665,0.5));
#30951=CARTESIAN_POINT('Ctrl Pts',(-7.9321719283244,15.6280424815024,98.1029310403532));
#30952=CARTESIAN_POINT('Ctrl Pts',(-7.88286802685643,15.8011193837335,98.3435819249719));
#30953=CARTESIAN_POINT('Ctrl Pts',(-7.6045369593422,15.809621013675,98.4565369103438));
#30954=CARTESIAN_POINT('Ctrl Pts',(-7.99314885854456,15.4140497422028,98.2878840681093));
#30955=CARTESIAN_POINT('Ctrl Pts',(-7.93830133829255,15.5743539404689,98.521498203427));
#30956=CARTESIAN_POINT('Ctrl Pts',(-7.67534747321984,15.5703297982934,98.6414834345645));
#30957=CARTESIAN_POINT('Ctrl Pts',(-8.07342544701438,15.1939319565419,98.4673409001115));
#30958=CARTESIAN_POINT('Ctrl Pts',(-8.01520601240624,15.337817496613,98.696680627363));
#30959=CARTESIAN_POINT('Ctrl Pts',(-7.76810813773555,15.3239231079797,98.8209468546291));
#30960=CARTESIAN_POINT('Ctrl Pts',(-8.27074145233702,14.7666413443144,98.786605947879));
#30961=CARTESIAN_POINT('Ctrl Pts',(-8.21126794551343,14.8786168342417,99.0079277681179));
#30962=CARTESIAN_POINT('Ctrl Pts',(-7.99520082055387,14.8449483706469,99.1402125820163));
#30963=CARTESIAN_POINT('Ctrl Pts',(-8.38626933427948,14.5585212736839,98.9284804941305));
#30964=CARTESIAN_POINT('Ctrl Pts',(-8.32817971805768,14.6543633819072,99.1468659074353));
#30965=CARTESIAN_POINT('Ctrl Pts',(-8.12783062814333,14.6113406338476,99.2820874488399));
#30966=CARTESIAN_POINT('Ctrl Pts',(-8.59454374091723,14.2490983667564,99.1108598027282));
#30967=CARTESIAN_POINT('Ctrl Pts',(-8.54319049921983,14.3207191002957,99.325486461323));
#30968=CARTESIAN_POINT('Ctrl Pts',(-8.3663329999394,14.2633935124894,99.4644671720462));
#30969=CARTESIAN_POINT('Ctrl Pts',(-8.67033161120472,14.1459038886755,99.1667281040791));
#30970=CARTESIAN_POINT('Ctrl Pts',(-8.62164751952555,14.2097749522394,99.380109563126));
#30971=CARTESIAN_POINT('Ctrl Pts',(-8.45303329796889,14.1472419030066,99.5203355960162));
#30972=CARTESIAN_POINT('Ctrl Pts',(-8.83156692003832,13.9454197645674,99.2638527346784));
#30973=CARTESIAN_POINT('Ctrl Pts',(-8.78941327154469,13.9945706318057,99.4749661095217));
#30974=CARTESIAN_POINT('Ctrl Pts',(-8.63728603612372,13.9213425720195,99.617460437482));
#30975=CARTESIAN_POINT('Ctrl Pts',(-8.91726990562776,13.8476543326374,99.3054399325309));
#30976=CARTESIAN_POINT('Ctrl Pts',(-8.87903935077148,13.8896197228001,99.515658214165));
#30977=CARTESIAN_POINT('Ctrl Pts',(-8.73513204645105,13.8110608770737,99.6590477275199));
#30978=CARTESIAN_POINT('Ctrl Pts',(-9.19086363206821,13.5622549366773,99.4071746058888));
#30979=CARTESIAN_POINT('Ctrl Pts',(-9.16559403544637,13.5845353846879,99.6148745113222));
#30980=CARTESIAN_POINT('Ctrl Pts',(-9.04717263343547,13.4887249880274,99.7607826165548));
#30981=CARTESIAN_POINT('Ctrl Pts',(-9.3986364390167,13.3806266657361,99.4435386777496));
#30982=CARTESIAN_POINT('Ctrl Pts',(-9.38579471648355,13.3899048404738,99.6506668510311));
#30983=CARTESIAN_POINT('Ctrl Pts',(-9.2837233434811,13.2830140381241,99.7971467765042));
#30984=CARTESIAN_POINT('Ctrl Pts',(-9.72568529812736,13.1438881211714,99.442502700397));
#30985=CARTESIAN_POINT('Ctrl Pts',(-9.73270657526614,13.1388413288334,99.6496543232892));
#30986=CARTESIAN_POINT('Ctrl Pts',(-9.65530926343492,13.0140082384199,99.7961107967627));
#30987=CARTESIAN_POINT('Ctrl Pts',(-9.83783804700205,13.0701625206814,99.4333242900205));
#30988=CARTESIAN_POINT('Ctrl Pts',(-9.85200497202217,13.0608830247369,99.6406660872407));
#30989=CARTESIAN_POINT('Ctrl Pts',(-9.78261877917289,12.9300742643075,99.7869323657969));
#30990=CARTESIAN_POINT('Ctrl Pts',(-10.0683558886233,12.9329789952414,99.3975703058088));
#30991=CARTESIAN_POINT('Ctrl Pts',(-10.0972665052523,12.9166588193608,99.6057238277679));
#30992=CARTESIAN_POINT('Ctrl Pts',(-10.0440416516022,12.7735790742388,99.751178303339));
#30993=CARTESIAN_POINT('Ctrl Pts',(-10.1878697697834,12.8690066204319,99.3706193994188));
#30994=CARTESIAN_POINT('Ctrl Pts',(-10.2246928633405,12.849751016337,99.5793392014517));
#30995=CARTESIAN_POINT('Ctrl Pts',(-10.1794547531643,12.7004270560128,99.7242273368565));
#30996=CARTESIAN_POINT('Ctrl Pts',(-10.5459796461518,12.6972294018582,99.2668124456041));
#30997=CARTESIAN_POINT('Ctrl Pts',(-10.6071137146221,12.6711601820488,99.4777222783443));
#30998=CARTESIAN_POINT('Ctrl Pts',(-10.5848323230216,12.5034972525403,99.6204201490476));
#30999=CARTESIAN_POINT('Ctrl Pts',(-10.7835265265761,12.6088970959964,99.1683014346687));
#31000=CARTESIAN_POINT('Ctrl Pts',(-10.8613053154178,12.581380754749,99.3809681438947));
#31001=CARTESIAN_POINT('Ctrl Pts',(-10.8532501470603,12.4015113889649,99.5219089068378));
#31002=CARTESIAN_POINT('Ctrl Pts',(-11.2574858404351,12.4740942697068,98.9266153300884));
#31003=CARTESIAN_POINT('Ctrl Pts',(-11.3667598443235,12.4485214406135,99.1450562468842));
#31004=CARTESIAN_POINT('Ctrl Pts',(-11.3879615918918,12.2445226500553,99.2802222813136));
#31005=CARTESIAN_POINT('Ctrl Pts',(-11.4955326995551,12.4278895523164,98.7818489409675));
#31006=CARTESIAN_POINT('Ctrl Pts',(-11.6208671315238,12.4060724976491,99.0032991843688));
#31007=CARTESIAN_POINT('Ctrl Pts',(-11.6560867497414,12.1897979679579,99.1354555654036));
#31008=CARTESIAN_POINT('Ctrl Pts',(-11.9602280353382,12.3732319398888,98.4637529209062));
#31009=CARTESIAN_POINT('Ctrl Pts',(-12.1153359231296,12.3624828687138,98.6931970175259));
#31010=CARTESIAN_POINT('Ctrl Pts',(-12.1787937287228,12.1229428480101,98.8173588681849));
#31011=CARTESIAN_POINT('Ctrl Pts',(-12.188933285124,12.3651447396865,98.2884223589317));
#31012=CARTESIAN_POINT('Ctrl Pts',(-12.3582902157324,12.3624926623483,98.5220290045064));
#31013=CARTESIAN_POINT('Ctrl Pts',(-12.4356699558978,12.1111989679492,98.6420342841727));
#31014=CARTESIAN_POINT('Ctrl Pts',(-12.4120365614475,12.3732750986753,98.1028819384482));
#31015=CARTESIAN_POINT('Ctrl Pts',(-12.5918835391586,12.3798704796615,98.3435328811866));
#31016=CARTESIAN_POINT('Ctrl Pts',(-12.6859819511989,12.1177859883826,98.4564865390546));
#31017=CARTESIAN_POINT('Ctrl Pts',(-8.00253786208647,15.4036548381006,98.292893219028));
#31018=CARTESIAN_POINT('Ctrl Pts',(-7.99178803978736,15.4350302895329,98.3104738971094));
#31019=CARTESIAN_POINT('Ctrl Pts',(-7.97797039659482,15.4651921241464,98.3279440199573));
#31020=CARTESIAN_POINT('Ctrl Pts',(-7.9612826368274,15.4937639830745,98.3450378047213));
#31021=CARTESIAN_POINT('Ctrl Pts',(-7.94610084002526,15.5197574155394,98.3605889853761));
#31022=CARTESIAN_POINT('Ctrl Pts',(-7.92854146285382,15.5444370156778,98.375828687269));
#31023=CARTESIAN_POINT('Ctrl Pts',(-7.90872785867543,15.5674910987838,98.3905567849321));
#31024=CARTESIAN_POINT('Ctrl Pts',(-7.89061591503621,15.5885652178644,98.4040199828634));
#31025=CARTESIAN_POINT('Ctrl Pts',(-7.8706186900642,15.6082816542381,98.4170556796548));
#31026=CARTESIAN_POINT('Ctrl Pts',(-7.84883313691036,15.6263606129814,98.4295110106493));
#31027=CARTESIAN_POINT('Ctrl Pts',(-7.82911718504767,15.642722092435,98.4407831002118));
#31028=CARTESIAN_POINT('Ctrl Pts',(-7.80793550877505,15.6577422663405,98.4515798544113));
#31029=CARTESIAN_POINT('Ctrl Pts',(-7.78537979191595,15.6711759357228,98.4617879668172));
#31030=CARTESIAN_POINT('Ctrl Pts',(-7.77424523654401,15.6778074223884,98.4668271679002));
#31031=CARTESIAN_POINT('Ctrl Pts',(-7.76277625253494,15.6840517008834,98.471722924588));
#31032=CARTESIAN_POINT('Ctrl Pts',(-7.75098709974896,15.6898756840048,98.4764616066469));
#31033=CARTESIAN_POINT('Origin',(-12.1669944801976,11.8680158329566,98.2808650734384));
#31034=CARTESIAN_POINT('Origin',(-7.52953032547042,15.2415935216047,100.));
#31035=CARTESIAN_POINT('Ctrl Pts',(-8.00253786221766,15.4036548377177,0.5));
#31036=CARTESIAN_POINT('Ctrl Pts',(-8.00221557868536,15.4045954850197,0.498951748855652));
#31037=CARTESIAN_POINT('Ctrl Pts',(-8.00189048816431,15.4055351740473,0.497903494266625));
#31038=CARTESIAN_POINT('Ctrl Pts',(-7.97222236614597,15.490471366956,0.40305758580859));
#31039=CARTESIAN_POINT('Ctrl Pts',(-7.92080050993637,15.5657442916618,0.310543821767294));
#31040=CARTESIAN_POINT('Ctrl Pts',(-7.82090726356976,15.6499070964475,0.195519413315074));
#31041=CARTESIAN_POINT('Ctrl Pts',(-7.78710654979053,15.6720322417137,0.163202546768292));
#31042=CARTESIAN_POINT('Ctrl Pts',(-7.75098709974896,15.6898756840048,0.134720657333156));
#31043=CARTESIAN_POINT('Origin',(-12.1688640072122,11.8709203002115,100.));
#31044=CARTESIAN_POINT('Ctrl Pts',(-12.5267717721302,12.2200650149237,0.134720657333156));
#31045=CARTESIAN_POINT('Ctrl Pts',(-12.4986401261759,12.2489027263445,0.163202546768228));
#31046=CARTESIAN_POINT('Ctrl Pts',(-12.4671528676167,12.2742120695494,0.195519413314942));
#31047=CARTESIAN_POINT('Ctrl Pts',(-12.3562405729316,12.3432084554757,0.310543821781225));
#31048=CARTESIAN_POINT('Ctrl Pts',(-12.2687615399374,12.3688529339454,0.403057585829754));
#31049=CARTESIAN_POINT('Ctrl Pts',(-12.1788144663217,12.3708222676705,0.497903494266489));
#31050=CARTESIAN_POINT('Ctrl Pts',(-12.1778203104527,12.37084106725,0.498951748856102));
#31051=CARTESIAN_POINT('Ctrl Pts',(-12.1768261106186,12.3708569011015,0.5));
#31052=CARTESIAN_POINT('Origin',(-12.2482946431511,16.8583313034371,0.5));
#31053=CARTESIAN_POINT('Ctrl Pts',(-3.12098026161583,17.2452472912803,98.4746163542476));
#31054=CARTESIAN_POINT('Ctrl Pts',(-2.89260432929213,17.4018708609359,98.3611663178014));
#31055=CARTESIAN_POINT('Ctrl Pts',(-2.75148341999934,17.2923597286537,98.1210629636544));
#31056=CARTESIAN_POINT('Ctrl Pts',(-2.73662446842834,16.9531805857873,98.830461882757));
#31057=CARTESIAN_POINT('Ctrl Pts',(-2.54985248945774,17.1146469822629,98.7002300650194));
#31058=CARTESIAN_POINT('Ctrl Pts',(-2.41148044251214,17.0285142699576,98.4769098403642));
#31059=CARTESIAN_POINT('Ctrl Pts',(-2.27713697342544,16.6926757665454,99.1602382875986));
#31060=CARTESIAN_POINT('Ctrl Pts',(-2.1262371091358,16.8482972498952,99.025549413826));
#31061=CARTESIAN_POINT('Ctrl Pts',(-2.00572321702971,16.7928860538427,98.8066848982746));
#31062=CARTESIAN_POINT('Ctrl Pts',(-1.48828850627704,16.4115930339874,99.5229830380901));
#31063=CARTESIAN_POINT('Ctrl Pts',(-1.38929487236062,16.5617976914248,99.3820315078356));
#31064=CARTESIAN_POINT('Ctrl Pts',(-1.31033409767418,16.5384526486055,99.1694296468622));
#31065=CARTESIAN_POINT('Ctrl Pts',(-1.20426376711567,16.3348109530474,99.6234913693268));
#31066=CARTESIAN_POINT('Ctrl Pts',(-1.12441622988599,16.4834764139428,99.4807426095521));
#31067=CARTESIAN_POINT('Ctrl Pts',(-1.06013194543873,16.4689116580449,99.2699379792856));
#31068=CARTESIAN_POINT('Ctrl Pts',(-0.610116136352994,16.2303876665528,
99.7608048122958));
#31069=CARTESIAN_POINT('Ctrl Pts',(-0.570592580096672,16.3774763782636,
99.6149071958598));
#31070=CARTESIAN_POINT('Ctrl Pts',(-0.536982386433238,16.3743182939755,
99.4072514211504));
#31071=CARTESIAN_POINT('Ctrl Pts',(-0.30439538532984,16.2034354627788,99.7966027452528));
#31072=CARTESIAN_POINT('Ctrl Pts',(-0.284158019240097,16.349880178516,99.6501526042807));
#31073=CARTESIAN_POINT('Ctrl Pts',(-0.267906895914236,16.3498931438339,
99.44304935477));
#31074=CARTESIAN_POINT('Ctrl Pts',(0.15523839877392,16.2036129415517,99.7963677642295));
#31075=CARTESIAN_POINT('Ctrl Pts',(0.144919417032302,16.3500605079967,99.6499229371978));
#31076=CARTESIAN_POINT('Ctrl Pts',(0.136629658481294,16.3500539600225,99.442814373581));
#31077=CARTESIAN_POINT('Ctrl Pts',(0.310467040971329,16.2104925143924,99.7872514480855));
#31078=CARTESIAN_POINT('Ctrl Pts',(0.289967609306312,16.3570649252483,99.6409952531274));
#31079=CARTESIAN_POINT('Ctrl Pts',(0.273250886060001,16.3562879072327,99.4336980572382));
#31080=CARTESIAN_POINT('Ctrl Pts',(0.616270430044837,16.2376016048274,99.7514230350795));
#31081=CARTESIAN_POINT('Ctrl Pts',(0.575332789986894,16.3846026904707,99.6059800049562));
#31082=CARTESIAN_POINT('Ctrl Pts',(0.542427079965384,16.3808502013102,99.3978696447402));
#31083=CARTESIAN_POINT('Ctrl Pts',(0.765900280741983,16.2576126110769,99.7250021223377));
#31084=CARTESIAN_POINT('Ctrl Pts',(0.715021742305763,16.4049628381998,99.580115086457));
#31085=CARTESIAN_POINT('Ctrl Pts',(0.67415035900587,16.3989804855663,99.3714487314956));
#31086=CARTESIAN_POINT('Ctrl Pts',(1.20584020603573,16.3354058480374,99.6227146850678));
#31087=CARTESIAN_POINT('Ctrl Pts',(1.12586029852619,16.4840769873469,99.4799874409063));
#31088=CARTESIAN_POINT('Ctrl Pts',(1.06152132333173,16.4694503946166,99.2691612949723));
#31089=CARTESIAN_POINT('Ctrl Pts',(1.4904584535125,16.4122197672618,99.5221656588587));
#31090=CARTESIAN_POINT('Ctrl Pts',(1.39131820921548,16.5624362368043,99.3812294188917));
#31091=CARTESIAN_POINT('Ctrl Pts',(1.31224595582737,16.5390201922298,99.1686122675856));
#31092=CARTESIAN_POINT('Ctrl Pts',(2.01683567706278,16.6000729369334,99.2797533468153));
#31093=CARTESIAN_POINT('Ctrl Pts',(1.87973999608435,16.7526185023833,99.1446071116388));
#31094=CARTESIAN_POINT('Ctrl Pts',(1.7762623025766,16.7090626239981,98.9261999569019));
#31095=CARTESIAN_POINT('Ctrl Pts',(2.2604912537429,16.7108289072469,99.1382521541666));
#31096=CARTESIAN_POINT('Ctrl Pts',(2.10526006254853,16.865041127594,99.0060308920483));
#31097=CARTESIAN_POINT('Ctrl Pts',(1.9912182095838,16.8092788783049,98.7846987631153));
#31098=CARTESIAN_POINT('Ctrl Pts',(2.71703050574192,16.9604363298062,98.8245648611896));
#31099=CARTESIAN_POINT('Ctrl Pts',(2.52562525529636,17.1167691877694,98.7003130263007));
#31100=CARTESIAN_POINT('Ctrl Pts',(2.39431788322584,17.035000481646,98.4710114710543));
#31101=CARTESIAN_POINT('Ctrl Pts',(2.92925959162593,17.0995673036633,98.6521093612491));
#31102=CARTESIAN_POINT('Ctrl Pts',(2.71988721110643,17.2571410628035,98.5320184901564));
#31103=CARTESIAN_POINT('Ctrl Pts',(2.58188146292243,17.1607523397371,98.298561852701));
#31104=CARTESIAN_POINT('Ctrl Pts',(3.12090206377706,17.2451878710232,98.4746887503082));
#31105=CARTESIAN_POINT('Ctrl Pts',(2.89253316440024,17.4018112264551,98.3612367156073));
#31106=CARTESIAN_POINT('Ctrl Pts',(2.75141424608767,17.2923060501388,98.1211353597149));
#31107=CARTESIAN_POINT('Ctrl Pts',(2.57985201764259,17.1655922764305,98.2928932196501));
#31108=CARTESIAN_POINT('Ctrl Pts',(2.60699083419288,17.1846569627295,98.3104738976888));
#31109=CARTESIAN_POINT('Ctrl Pts',(2.635898223901,17.2009365925282,98.3279440204933));
#31110=CARTESIAN_POINT('Ctrl Pts',(2.66619302242479,17.2142428927914,98.3450378052143));
#31111=CARTESIAN_POINT('Ctrl Pts',(2.69375391028467,17.2263483850626,98.3605889858378));
#31112=CARTESIAN_POINT('Ctrl Pts',(2.72246604979616,17.2359934579821,98.3758286876993));
#31113=CARTESIAN_POINT('Ctrl Pts',(2.75204644232091,17.2429984586142,98.3905567853312));
#31114=CARTESIAN_POINT('Ctrl Pts',(2.77908636891128,17.2494018456788,98.40401998324));
#31115=CARTESIAN_POINT('Ctrl Pts',(2.80685349426263,17.2535987038001,98.4170556800087));
#31116=CARTESIAN_POINT('Ctrl Pts',(2.83510492229913,17.2554196617626,98.4295110109802));
#31117=CARTESIAN_POINT('Ctrl Pts',(2.86067249873503,17.2570676309142,98.4407831005269));
#31118=CARTESIAN_POINT('Ctrl Pts',(2.88663747150523,17.256768929892,98.45157985471));
#31119=CARTESIAN_POINT('Ctrl Pts',(2.91278154249718,17.2543790789575,98.4617879670986));
#31120=CARTESIAN_POINT('Ctrl Pts',(2.9256874768416,17.2531993369325,98.4668271680826));
#31121=CARTESIAN_POINT('Ctrl Pts',(2.93863637438248,17.2515097647149,98.4717229246763));
#31122=CARTESIAN_POINT('Ctrl Pts',(2.95159725048241,17.2492919759318,98.4764616066469));
#31123=CARTESIAN_POINT('Ctrl Pts',(-2.95159725048241,17.2492919759318,98.4764616066469));
#31124=CARTESIAN_POINT('Ctrl Pts',(-2.92468746478162,17.2538966199714,98.4666230035039));
#31125=CARTESIAN_POINT('Ctrl Pts',(-2.89776866146892,17.2562336662028,98.4560730110185));
#31126=CARTESIAN_POINT('Ctrl Pts',(-2.8711410682296,17.256440045183,98.4449543865007));
#31127=CARTESIAN_POINT('Ctrl Pts',(-2.84186545383984,17.256666947832,98.4327300536064));
#31128=CARTESIAN_POINT('Ctrl Pts',(-2.81294183067497,17.2543190646552,98.4198183681925));
#31129=CARTESIAN_POINT('Ctrl Pts',(-2.78470495960319,17.2495916469058,98.4064090535574));
#31130=CARTESIAN_POINT('Ctrl Pts',(-2.75441171242718,17.2445199506112,98.3920231932519));
#31131=CARTESIAN_POINT('Ctrl Pts',(-2.7249081422635,17.2367102069049,98.3770645838805));
#31132=CARTESIAN_POINT('Ctrl Pts',(-2.69654342028693,17.2264059478107,98.3617674909993));
#31133=CARTESIAN_POINT('Ctrl Pts',(-2.66333319608111,17.2143414278385,98.343857219053));
#31134=CARTESIAN_POINT('Ctrl Pts',(-2.63168331068654,17.1988577415015,98.3254829406024));
#31135=CARTESIAN_POINT('Ctrl Pts',(-2.60208076577926,17.1803381173616,98.3070206560147));
#31136=CARTESIAN_POINT('Ctrl Pts',(-2.59453756219189,17.1756190198757,98.3023161695671));
#31137=CARTESIAN_POINT('Ctrl Pts',(-2.58712702115892,17.1707027521152,98.2976059687736));
#31138=CARTESIAN_POINT('Ctrl Pts',(-2.57985673374437,17.1655955893937,98.2928962747547));
#31139=CARTESIAN_POINT('Origin',(2.86726590046863,16.7564550623337,100.));
#31140=CARTESIAN_POINT('Ctrl Pts',(2.57985201635105,17.1655922755232,0.5));
#31141=CARTESIAN_POINT('Ctrl Pts',(2.58066564781748,17.1661638416689,0.498951748855505));
#31142=CARTESIAN_POINT('Ctrl Pts',(2.58148098692646,17.1667329826481,0.497903494266865));
#31143=CARTESIAN_POINT('Ctrl Pts',(2.6554072434575,17.2180093215973,0.403057585720023));
#31144=CARTESIAN_POINT('Ctrl Pts',(2.74125271406851,17.2486813881449,0.310543821709137));
#31145=CARTESIAN_POINT('Ctrl Pts',(2.87153770337927,17.2580547504886,0.195519413316264));
#31146=CARTESIAN_POINT('Ctrl Pts',(2.91188788934173,17.2560868079356,0.163202546768814));
#31147=CARTESIAN_POINT('Ctrl Pts',(2.95159725048241,17.2492919759318,0.13472065733316));
#31148=CARTESIAN_POINT('Origin',(-2.86726590046863,16.7564550623337,100.));
#31149=CARTESIAN_POINT('Ctrl Pts',(-2.95159725048241,17.2492919759318,0.134720657333159));
#31150=CARTESIAN_POINT('Ctrl Pts',(-2.91188788934176,17.2560868079356,0.163202546768789));
#31151=CARTESIAN_POINT('Ctrl Pts',(-2.87153770337939,17.2580547504885,0.19551941331617));
#31152=CARTESIAN_POINT('Ctrl Pts',(-2.74125271406348,17.2486813881446,0.310543821713542));
#31153=CARTESIAN_POINT('Ctrl Pts',(-2.65540724345347,17.2180093215945,0.403057585726612));
#31154=CARTESIAN_POINT('Ctrl Pts',(-2.58148098692643,17.1667329826481,0.497903494266832));
#31155=CARTESIAN_POINT('Ctrl Pts',(-2.58066564781746,17.1661638416689,0.49895174885553));
#31156=CARTESIAN_POINT('Ctrl Pts',(-2.57985201635105,17.1655922755232,0.5));
#31157=CARTESIAN_POINT('Origin',(0.,20.8380434782609,0.5));
#31158=CARTESIAN_POINT('',(0.,0.,0.));
#31159=CARTESIAN_POINT('Origin',(0.,15.,-9.));
#31160=CARTESIAN_POINT('',(-13.8985,-1.70207535379495E-15,-9.));
#31161=CARTESIAN_POINT('Origin',(0.,0.,-9.));
#31162=CARTESIAN_POINT('',(4.5,-5.51091059616309E-16,-9.));
#31163=CARTESIAN_POINT('Origin',(0.,0.,-9.));
#31164=CARTESIAN_POINT('Origin',(0.,15.,2.44929359829471E-16));
#31165=CARTESIAN_POINT('',(14.5,-1.77573785876366E-15,2.08166817117217E-16));
#31166=CARTESIAN_POINT('Origin',(0.,0.,2.16840434497101E-16));
#31167=CARTESIAN_POINT('',(-4.7583302491977,4.7583302491977,0.));
#31168=CARTESIAN_POINT('',(-6.5,3.75277674973257,0.));
#31169=CARTESIAN_POINT('',(-3.67669907207811E-16,7.50555349946513,0.));
#31170=CARTESIAN_POINT('',(-3.75277674973257,6.5,0.));
#31171=CARTESIAN_POINT('',(-3.75277674973257,6.5,0.));
#31172=CARTESIAN_POINT('',(-1.7416697508023,6.5,0.));
#31173=CARTESIAN_POINT('',(3.75277674973257,6.5,0.));
#31174=CARTESIAN_POINT('',(-3.67669907207811E-16,7.50555349946513,0.));
#31175=CARTESIAN_POINT('',(-3.67669907207811E-16,7.50555349946513,0.));
#31176=CARTESIAN_POINT('',(1.7416697508023,6.5,0.));
#31177=CARTESIAN_POINT('',(6.5,3.75277674973257,0.));
#31178=CARTESIAN_POINT('',(3.75277674973257,6.5,0.));
#31179=CARTESIAN_POINT('',(3.75277674973257,6.5,0.));
#31180=CARTESIAN_POINT('',(4.7583302491977,4.7583302491977,0.));
#31181=CARTESIAN_POINT('',(7.50555349946514,1.02623325203886E-15,0.));
#31182=CARTESIAN_POINT('',(6.5,3.75277674973257,0.));
#31183=CARTESIAN_POINT('',(6.5,3.75277674973257,0.));
#31184=CARTESIAN_POINT('',(6.5,1.7416697508023,0.));
#31185=CARTESIAN_POINT('',(6.5,-3.75277674973257,0.));
#31186=CARTESIAN_POINT('',(7.50555349946514,0.,2.44929359829471E-16));
#31187=CARTESIAN_POINT('',(7.50555349946514,1.02623325203886E-15,0.));
#31188=CARTESIAN_POINT('',(6.5,-1.7416697508023,0.));
#31189=CARTESIAN_POINT('',(3.75277674973257,-6.5,0.));
#31190=CARTESIAN_POINT('',(6.5,-3.75277674973257,0.));
#31191=CARTESIAN_POINT('',(6.5,-3.75277674973257,0.));
#31192=CARTESIAN_POINT('',(4.7583302491977,-4.7583302491977,0.));
#31193=CARTESIAN_POINT('',(-1.19266633607575E-15,-7.50555349946513,0.));
#31194=CARTESIAN_POINT('',(3.75277674973257,-6.5,0.));
#31195=CARTESIAN_POINT('',(3.75277674973257,-6.5,0.));
#31196=CARTESIAN_POINT('',(1.7416697508023,-6.5,0.));
#31197=CARTESIAN_POINT('',(-3.75277674973256,-6.5,0.));
#31198=CARTESIAN_POINT('',(-1.19266633607575E-15,-7.50555349946513,0.));
#31199=CARTESIAN_POINT('',(-1.19266633607575E-15,-7.50555349946513,0.));
#31200=CARTESIAN_POINT('',(-1.7416697508023,-6.5,0.));
#31201=CARTESIAN_POINT('',(-6.5,-3.75277674973257,0.));
#31202=CARTESIAN_POINT('',(-3.75277674973256,-6.5,0.));
#31203=CARTESIAN_POINT('',(-3.75277674973256,-6.5,0.));
#31204=CARTESIAN_POINT('',(-4.75833024919769,-4.75833024919771,0.));
#31205=CARTESIAN_POINT('',(-7.50555349946513,1.69369577295829E-15,0.));
#31206=CARTESIAN_POINT('',(-6.5,-3.75277674973257,0.));
#31207=CARTESIAN_POINT('',(-6.5,-3.75277674973257,0.));
#31208=CARTESIAN_POINT('',(-6.5,-1.74166975080229,0.));
#31209=CARTESIAN_POINT('',(-6.5,3.75277674973257,0.));
#31210=CARTESIAN_POINT('',(-7.50555349946513,1.69369577295829E-15,0.));
#31211=CARTESIAN_POINT('',(-7.50555349946513,1.69369577295829E-15,0.));
#31212=CARTESIAN_POINT('',(-6.5,1.7416697508023,0.));
#31213=CARTESIAN_POINT('',(-3.75277674973257,6.5,0.));
#31214=CARTESIAN_POINT('',(-6.5,3.75277674973257,0.));
#31215=CARTESIAN_POINT('Origin',(3.75277674973257,-6.5,-7.));
#31216=CARTESIAN_POINT('',(6.5,-1.7416697508023,-7.));
#31217=CARTESIAN_POINT('',(7.50555349946514,1.02623325203886E-15,-7.));
#31218=CARTESIAN_POINT('',(3.75277674973257,-6.5,-7.));
#31219=CARTESIAN_POINT('',(6.5,-1.7416697508023,-7.));
#31220=CARTESIAN_POINT('',(7.50555349946514,1.02623325203886E-15,-7.));
#31221=CARTESIAN_POINT('Origin',(-3.75277674973256,-6.5,-7.));
#31222=CARTESIAN_POINT('',(1.7416697508023,-6.5,-7.));
#31223=CARTESIAN_POINT('',(3.75277674973257,-6.5,-7.));
#31224=CARTESIAN_POINT('',(-3.75277674973256,-6.5,-7.));
#31225=CARTESIAN_POINT('',(1.7416697508023,-6.5,-7.));
#31226=CARTESIAN_POINT('',(3.75277674973257,-6.5,-7.));
#31227=CARTESIAN_POINT('Origin',(-7.50555349946513,1.69369577295829E-15,
-7.));
#31228=CARTESIAN_POINT('',(-4.75833024919769,-4.75833024919771,-7.));
#31229=CARTESIAN_POINT('',(-3.75277674973256,-6.5,-7.));
#31230=CARTESIAN_POINT('',(-7.50555349946513,1.69369577295829E-15,-7.));
#31231=CARTESIAN_POINT('',(-4.7583302491977,-4.75833024919771,-7.));
#31232=CARTESIAN_POINT('',(-3.75277674973256,-6.5,-7.));
#31233=CARTESIAN_POINT('Origin',(-3.75277674973257,6.5,-7.));
#31234=CARTESIAN_POINT('',(-4.7583302491977,4.7583302491977,-7.));
#31235=CARTESIAN_POINT('',(-4.7583302491977,4.7583302491977,-7.));
#31236=CARTESIAN_POINT('',(-3.75277674973257,6.5,-7.));
#31237=CARTESIAN_POINT('',(-3.75277674973257,6.5,-7.));
#31238=CARTESIAN_POINT('',(-3.75277674973257,6.5,-7.));
#31239=CARTESIAN_POINT('Origin',(3.75277674973257,6.5,-7.));
#31240=CARTESIAN_POINT('',(-1.7416697508023,6.5,-7.));
#31241=CARTESIAN_POINT('',(3.75277674973257,6.5,-7.));
#31242=CARTESIAN_POINT('',(-1.7416697508023,6.5,-7.));
#31243=CARTESIAN_POINT('Origin',(7.50555349946514,1.02623325203886E-15,
-7.));
#31244=CARTESIAN_POINT('',(4.7583302491977,4.7583302491977,-7.));
#31245=CARTESIAN_POINT('',(3.75277674973257,6.5,-7.));
#31246=CARTESIAN_POINT('',(7.50555349946514,1.02623325203886E-15,-7.));
#31247=CARTESIAN_POINT('',(4.7583302491977,4.7583302491977,-7.));
#31248=CARTESIAN_POINT('',(3.75277674973257,6.5,-7.));
#31249=CARTESIAN_POINT('Origin',(0.,0.,0.));
#31250=CARTESIAN_POINT('',(4.5,0.,-8.15470053837925));
#31251=CARTESIAN_POINT('',(-4.5,-5.51091059616309E-16,-8.15470053837925));
#31252=CARTESIAN_POINT('Origin',(0.,0.,-8.15470053837925));
#31253=CARTESIAN_POINT('Origin',(0.,0.,-8.15470053837925));
#31254=CARTESIAN_POINT('',(4.5,-5.51091059616309E-16,0.));
#31255=CARTESIAN_POINT('Origin',(0.,0.,0.));
#31256=CARTESIAN_POINT('',(-15.,0.,-0.5));
#31257=CARTESIAN_POINT('',(15.,-1.83697019872103E-15,-0.5));
#31258=CARTESIAN_POINT('Origin',(0.,0.,-0.5));
#31259=CARTESIAN_POINT('Origin',(0.,0.,-0.5));
#31260=CARTESIAN_POINT('',(-15.,-1.83697019872103E-15,-7.89850000000002));
#31261=CARTESIAN_POINT('',(-15.,-1.83697019872103E-15,0.));
#31262=CARTESIAN_POINT('Origin',(0.,0.,-7.89850000000002));
#31263=CARTESIAN_POINT('Origin',(0.,0.,-7.));
#31264=CARTESIAN_POINT('',(-7.50555349946513,1.69369577295829E-15,-7.));
#31265=CARTESIAN_POINT('',(-6.5,-1.74166975080229,-7.));
#31266=CARTESIAN_POINT('',(-7.50555349946513,1.69369577295829E-15,-7.));
#31267=CARTESIAN_POINT('',(-6.5,-3.75277674973257,-7.));
#31268=CARTESIAN_POINT('',(-6.5,3.75277674973257,-7.));
#31269=CARTESIAN_POINT('',(-6.5,-3.75277674973257,-7.));
#31270=CARTESIAN_POINT('',(-1.7416697508023,-6.5,-7.));
#31271=CARTESIAN_POINT('',(-3.75277674973256,-6.5,-7.));
#31272=CARTESIAN_POINT('',(-1.19266633607575E-15,-7.50555349946513,-7.));
#31273=CARTESIAN_POINT('',(-6.5,-3.75277674973257,-7.));
#31274=CARTESIAN_POINT('',(-1.19266633607575E-15,-7.50555349946513,-7.));
#31275=CARTESIAN_POINT('',(4.75833024919771,-4.7583302491977,-7.));
#31276=CARTESIAN_POINT('',(3.75277674973257,-6.5,-7.));
#31277=CARTESIAN_POINT('',(6.5,-3.75277674973257,-7.));
#31278=CARTESIAN_POINT('',(-1.19266633607575E-15,-7.50555349946513,-7.));
#31279=CARTESIAN_POINT('',(6.5,-3.75277674973257,-7.));
#31280=CARTESIAN_POINT('',(6.5,1.7416697508023,-7.));
#31281=CARTESIAN_POINT('',(7.50555349946514,1.02623325203886E-15,-7.));
#31282=CARTESIAN_POINT('',(6.5,3.75277674973257,-7.));
#31283=CARTESIAN_POINT('',(6.5,-3.75277674973257,-7.));
#31284=CARTESIAN_POINT('',(6.5,3.75277674973257,-7.));
#31285=CARTESIAN_POINT('',(1.7416697508023,6.5,-7.));
#31286=CARTESIAN_POINT('',(3.75277674973257,6.5,-7.));
#31287=CARTESIAN_POINT('',(-3.67669907207811E-16,7.50555349946513,-7.));
#31288=CARTESIAN_POINT('',(6.5,3.75277674973257,-7.));
#31289=CARTESIAN_POINT('',(-3.67669907207811E-16,7.50555349946513,-7.));
#31290=CARTESIAN_POINT('',(-6.5,3.75277674973257,-7.));
#31291=CARTESIAN_POINT('',(-3.67669907207811E-16,7.50555349946513,-7.));
#31292=CARTESIAN_POINT('',(-6.5,1.7416697508023,-7.));
#31293=CARTESIAN_POINT('',(-6.5,3.75277674973257,-7.));
#31294=CARTESIAN_POINT('',(-3.75277674973257,6.5,-7.));
#31295=CARTESIAN_POINT('',(-6.50000000000001,-7.9602041944578E-16,-7.));
#31296=CARTESIAN_POINT('Origin',(0.,0.,-7.));
#31297=CARTESIAN_POINT('Origin',(3.75277674973257,-6.5,-7.));
#31298=CARTESIAN_POINT('',(4.75833024919771,-4.7583302491977,-7.));
#31299=CARTESIAN_POINT('Origin',(-3.75277674973256,-6.5,-7.));
#31300=CARTESIAN_POINT('',(-1.7416697508023,-6.5,-7.));
#31301=CARTESIAN_POINT('Origin',(-7.50555349946513,1.69369577295829E-15,
-7.));
#31302=CARTESIAN_POINT('',(-6.5,-1.74166975080229,-7.));
#31303=CARTESIAN_POINT('',(-7.50555349946513,1.69369577295829E-15,-7.));
#31304=CARTESIAN_POINT('Origin',(-3.75277674973257,6.5,-7.));
#31305=CARTESIAN_POINT('',(-6.5,1.7416697508023,-7.));
#31306=CARTESIAN_POINT('Origin',(3.75277674973257,6.5,-7.));
#31307=CARTESIAN_POINT('',(1.7416697508023,6.5,-7.));
#31308=CARTESIAN_POINT('Origin',(7.50555349946514,1.02623325203886E-15,
-7.));
#31309=CARTESIAN_POINT('',(6.5,1.7416697508023,-7.));
#31310=CARTESIAN_POINT('Origin',(6.5,-3.75277674973257,-7.));
#31311=CARTESIAN_POINT('',(6.5,3.75277674973257,-7.));
#31312=CARTESIAN_POINT('Origin',(6.5,3.75277674973257,-7.));
#31313=CARTESIAN_POINT('Origin',(6.5,3.75277674973257,-7.));
#31314=CARTESIAN_POINT('',(-3.67669907207811E-16,7.50555349946513,-7.));
#31315=CARTESIAN_POINT('Origin',(-3.67669907207811E-16,7.50555349946513,
-7.));
#31316=CARTESIAN_POINT('Origin',(-6.5,3.75277674973257,-7.));
#31317=CARTESIAN_POINT('',(-6.5,3.75277674973257,-7.));
#31318=CARTESIAN_POINT('Origin',(-3.67669907207811E-16,7.50555349946513,
-7.));
#31319=CARTESIAN_POINT('Origin',(-6.5,3.75277674973257,-7.));
#31320=CARTESIAN_POINT('',(-6.5,-3.75277674973257,-7.));
#31321=CARTESIAN_POINT('Origin',(-6.5,-3.75277674973257,-7.));
#31322=CARTESIAN_POINT('Origin',(-6.5,-3.75277674973257,-7.));
#31323=CARTESIAN_POINT('',(-1.19266633607575E-15,-7.50555349946513,-7.));
#31324=CARTESIAN_POINT('Origin',(-1.19266633607575E-15,-7.50555349946513,
-7.));
#31325=CARTESIAN_POINT('Origin',(-1.19266633607575E-15,-7.50555349946513,
-7.));
#31326=CARTESIAN_POINT('',(6.5,-3.75277674973257,-7.));
#31327=CARTESIAN_POINT('Origin',(6.5,-3.75277674973257,-7.));
#31328=CARTESIAN_POINT('Origin',(0.,0.,-7.));
#31329=CARTESIAN_POINT('',(-6.50000000000001,-7.9602041944578E-16,-7.));
#31330=CARTESIAN_POINT('Origin',(0.,0.,-0.5));
#31331=CARTESIAN_POINT('Origin',(14.5,-1.77573785876366E-15,-0.5));
#31332=CARTESIAN_POINT('Origin',(0.,0.,-9.));
#31333=CARTESIAN_POINT('',(-13.8985,-1.70207535379495E-15,-9.));
#31334=CARTESIAN_POINT('',(0.,0.,0.));
#31335=CARTESIAN_POINT('Ctrl Pts',(0.,0.,13.55));
#31336=CARTESIAN_POINT('Ctrl Pts',(-5.61259377015544,0.0749999999999998,
13.55));
#31337=CARTESIAN_POINT('Ctrl Pts',(-9.58129688507772,0.15,9.58129688507772));
#31338=CARTESIAN_POINT('Ctrl Pts',(-13.55,0.225,5.61259377015544));
#31339=CARTESIAN_POINT('Ctrl Pts',(-13.55,0.299999999999999,8.29698206422332E-16));
#31340=CARTESIAN_POINT('Ctrl Pts',(-13.55,0.374999999999999,-5.61259377015544));
#31341=CARTESIAN_POINT('Ctrl Pts',(-9.58129688507772,0.449999999999999,
-9.58129688507772));
#31342=CARTESIAN_POINT('Ctrl Pts',(-5.61259377015544,0.524999999999999,
-13.55));
#31343=CARTESIAN_POINT('Ctrl Pts',(-1.65939641284466E-15,0.599999999999999,
-13.55));
#31344=CARTESIAN_POINT('Ctrl Pts',(5.61259377015543,0.674999999999998,-13.55));
#31345=CARTESIAN_POINT('Ctrl Pts',(9.58129688507772,0.749999999999998,-9.58129688507772));
#31346=CARTESIAN_POINT('Ctrl Pts',(13.55,0.824999999999998,-5.61259377015545));
#31347=CARTESIAN_POINT('Ctrl Pts',(13.55,0.899999999999998,-2.489094619267E-15));
#31348=CARTESIAN_POINT('Ctrl Pts',(13.55,0.974999999999998,5.61259377015544));
#31349=CARTESIAN_POINT('Ctrl Pts',(9.58129688507772,1.05,9.58129688507772));
#31350=CARTESIAN_POINT('Ctrl Pts',(5.61259377015545,1.125,13.55));
#31351=CARTESIAN_POINT('Ctrl Pts',(0.,1.2,13.55));
#31352=CARTESIAN_POINT('Ctrl Pts',(-5.61259377015544,1.275,13.55));
#31353=CARTESIAN_POINT('Ctrl Pts',(-9.58129688507772,1.35,9.58129688507772));
#31354=CARTESIAN_POINT('Ctrl Pts',(-13.55,1.425,5.61259377015544));
#31355=CARTESIAN_POINT('Ctrl Pts',(-13.55,1.5,8.29698206422332E-16));
#31356=CARTESIAN_POINT('Ctrl Pts',(-13.55,1.575,-5.61259377015544));
#31357=CARTESIAN_POINT('Ctrl Pts',(-9.58129688507772,1.65,-9.58129688507772));
#31358=CARTESIAN_POINT('Ctrl Pts',(-5.61259377015544,1.725,-13.55));
#31359=CARTESIAN_POINT('Ctrl Pts',(-1.65939641284466E-15,1.8,-13.55));
#31360=CARTESIAN_POINT('Ctrl Pts',(5.61259377015543,1.875,-13.55));
#31361=CARTESIAN_POINT('Ctrl Pts',(9.58129688507772,1.95,-9.58129688507772));
#31362=CARTESIAN_POINT('Ctrl Pts',(13.55,2.025,-5.61259377015545));
#31363=CARTESIAN_POINT('Ctrl Pts',(13.55,2.1,-2.489094619267E-15));
#31364=CARTESIAN_POINT('Ctrl Pts',(13.55,2.17499999999999,5.61259377015544));
#31365=CARTESIAN_POINT('Ctrl Pts',(9.58129688507772,2.25,9.58129688507772));
#31366=CARTESIAN_POINT('Ctrl Pts',(5.61259377015545,2.32499999999999,13.55));
#31367=CARTESIAN_POINT('Ctrl Pts',(0.,2.39999999999999,13.55));
#31368=CARTESIAN_POINT('Ctrl Pts',(-5.61259377015544,2.47499999999999,13.55));
#31369=CARTESIAN_POINT('Ctrl Pts',(-9.58129688507772,2.54999999999999,9.58129688507772));
#31370=CARTESIAN_POINT('Ctrl Pts',(-13.55,2.62499999999999,5.61259377015544));
#31371=CARTESIAN_POINT('Ctrl Pts',(-13.55,2.69999999999999,8.29698206422332E-16));
#31372=CARTESIAN_POINT('Ctrl Pts',(-13.55,2.77499999999999,-5.61259377015544));
#31373=CARTESIAN_POINT('Ctrl Pts',(-9.58129688507772,2.84999999999999,-9.58129688507772));
#31374=CARTESIAN_POINT('Ctrl Pts',(-5.61259377015544,2.92499999999999,-13.55));
#31375=CARTESIAN_POINT('Ctrl Pts',(-1.65939641284466E-15,2.99999999999999,
-13.55));
#31376=CARTESIAN_POINT('Ctrl Pts',(5.61259377015543,3.07499999999999,-13.55));
#31377=CARTESIAN_POINT('Ctrl Pts',(9.58129688507772,3.14999999999999,-9.58129688507772));
#31378=CARTESIAN_POINT('Ctrl Pts',(13.55,3.22499999999999,-5.61259377015545));
#31379=CARTESIAN_POINT('Ctrl Pts',(13.55,3.29999999999999,-2.489094619267E-15));
#31380=CARTESIAN_POINT('Ctrl Pts',(13.55,3.37499999999999,5.61259377015544));
#31381=CARTESIAN_POINT('Ctrl Pts',(9.58129688507772,3.44999999999999,9.58129688507772));
#31382=CARTESIAN_POINT('Ctrl Pts',(5.61259377015545,3.52499999999999,13.55));
#31383=CARTESIAN_POINT('Ctrl Pts',(0.,3.59999999999999,13.55));
#31384=CARTESIAN_POINT('Ctrl Pts',(-5.61259377015544,3.67499999999999,13.55));
#31385=CARTESIAN_POINT('Ctrl Pts',(-9.58129688507772,3.74999999999999,9.58129688507772));
#31386=CARTESIAN_POINT('Ctrl Pts',(-13.55,3.82499999999999,5.61259377015544));
#31387=CARTESIAN_POINT('Ctrl Pts',(-13.55,3.89999999999999,8.29698206422332E-16));
#31388=CARTESIAN_POINT('Ctrl Pts',(-13.55,3.97499999999999,-5.61259377015544));
#31389=CARTESIAN_POINT('Ctrl Pts',(-9.58129688507772,4.04999999999999,-9.58129688507772));
#31390=CARTESIAN_POINT('Ctrl Pts',(-5.61259377015544,4.12499999999999,-13.55));
#31391=CARTESIAN_POINT('Ctrl Pts',(-1.65939641284466E-15,4.19999999999999,
-13.55));
#31392=CARTESIAN_POINT('Ctrl Pts',(5.61259377015543,4.27499999999999,-13.55));
#31393=CARTESIAN_POINT('Ctrl Pts',(9.58129688507772,4.34999999999999,-9.58129688507772));
#31394=CARTESIAN_POINT('Ctrl Pts',(13.55,4.42499999999999,-5.61259377015545));
#31395=CARTESIAN_POINT('Ctrl Pts',(13.55,4.49999999999999,-2.489094619267E-15));
#31396=CARTESIAN_POINT('Ctrl Pts',(13.55,4.57499999999999,5.61259377015544));
#31397=CARTESIAN_POINT('Ctrl Pts',(9.58129688507772,4.64999999999999,9.58129688507772));
#31398=CARTESIAN_POINT('Ctrl Pts',(5.61259377015545,4.72499999999999,13.55));
#31399=CARTESIAN_POINT('Ctrl Pts',(0.,4.79999999999999,13.55));
#31400=CARTESIAN_POINT('Ctrl Pts',(0.,0.351471862576143,13.55));
#31401=CARTESIAN_POINT('Ctrl Pts',(-5.61259377015544,0.426471862576143,
13.55));
#31402=CARTESIAN_POINT('Ctrl Pts',(-9.58129688507772,0.501471862576143,
9.58129688507772));
#31403=CARTESIAN_POINT('Ctrl Pts',(-13.55,0.576471862576143,5.61259377015544));
#31404=CARTESIAN_POINT('Ctrl Pts',(-13.55,0.651471862576142,8.29698206422332E-16));
#31405=CARTESIAN_POINT('Ctrl Pts',(-13.55,0.726471862576142,-5.61259377015544));
#31406=CARTESIAN_POINT('Ctrl Pts',(-9.58129688507772,0.801471862576142,
-9.58129688507772));
#31407=CARTESIAN_POINT('Ctrl Pts',(-5.61259377015544,0.876471862576142,
-13.55));
#31408=CARTESIAN_POINT('Ctrl Pts',(-1.65939641284466E-15,0.951471862576142,
-13.55));
#31409=CARTESIAN_POINT('Ctrl Pts',(5.61259377015544,1.02647186257614,-13.55));
#31410=CARTESIAN_POINT('Ctrl Pts',(9.58129688507772,1.10147186257614,-9.58129688507772));
#31411=CARTESIAN_POINT('Ctrl Pts',(13.55,1.17647186257614,-5.61259377015545));
#31412=CARTESIAN_POINT('Ctrl Pts',(13.55,1.25147186257614,-2.489094619267E-15));
#31413=CARTESIAN_POINT('Ctrl Pts',(13.55,1.32647186257614,5.61259377015544));
#31414=CARTESIAN_POINT('Ctrl Pts',(9.58129688507772,1.40147186257614,9.58129688507772));
#31415=CARTESIAN_POINT('Ctrl Pts',(5.61259377015545,1.47647186257614,13.55));
#31416=CARTESIAN_POINT('Ctrl Pts',(0.,1.55147186257614,13.55));
#31417=CARTESIAN_POINT('Ctrl Pts',(-5.61259377015544,1.62647186257614,13.55));
#31418=CARTESIAN_POINT('Ctrl Pts',(-9.58129688507772,1.70147186257614,9.58129688507772));
#31419=CARTESIAN_POINT('Ctrl Pts',(-13.55,1.77647186257614,5.61259377015544));
#31420=CARTESIAN_POINT('Ctrl Pts',(-13.55,1.85147186257614,8.29698206422332E-16));
#31421=CARTESIAN_POINT('Ctrl Pts',(-13.55,1.92647186257614,-5.61259377015544));
#31422=CARTESIAN_POINT('Ctrl Pts',(-9.58129688507772,2.00147186257614,-9.58129688507772));
#31423=CARTESIAN_POINT('Ctrl Pts',(-5.61259377015544,2.07647186257614,-13.55));
#31424=CARTESIAN_POINT('Ctrl Pts',(-1.65939641284466E-15,2.15147186257614,
-13.55));
#31425=CARTESIAN_POINT('Ctrl Pts',(5.61259377015544,2.22647186257614,-13.55));
#31426=CARTESIAN_POINT('Ctrl Pts',(9.58129688507772,2.30147186257614,-9.58129688507772));
#31427=CARTESIAN_POINT('Ctrl Pts',(13.55,2.37647186257614,-5.61259377015545));
#31428=CARTESIAN_POINT('Ctrl Pts',(13.55,2.45147186257614,-2.489094619267E-15));
#31429=CARTESIAN_POINT('Ctrl Pts',(13.55,2.52647186257614,5.61259377015544));
#31430=CARTESIAN_POINT('Ctrl Pts',(9.58129688507772,2.60147186257614,9.58129688507772));
#31431=CARTESIAN_POINT('Ctrl Pts',(5.61259377015545,2.67647186257614,13.55));
#31432=CARTESIAN_POINT('Ctrl Pts',(0.,2.75147186257614,13.55));
#31433=CARTESIAN_POINT('Ctrl Pts',(-5.61259377015544,2.82647186257614,13.55));
#31434=CARTESIAN_POINT('Ctrl Pts',(-9.58129688507772,2.90147186257614,9.58129688507772));
#31435=CARTESIAN_POINT('Ctrl Pts',(-13.55,2.97647186257614,5.61259377015544));
#31436=CARTESIAN_POINT('Ctrl Pts',(-13.55,3.05147186257614,8.29698206422332E-16));
#31437=CARTESIAN_POINT('Ctrl Pts',(-13.55,3.12647186257614,-5.61259377015544));
#31438=CARTESIAN_POINT('Ctrl Pts',(-9.58129688507772,3.20147186257614,-9.58129688507772));
#31439=CARTESIAN_POINT('Ctrl Pts',(-5.61259377015544,3.27647186257614,-13.55));
#31440=CARTESIAN_POINT('Ctrl Pts',(-1.65939641284466E-15,3.35147186257614,
-13.55));
#31441=CARTESIAN_POINT('Ctrl Pts',(5.61259377015544,3.42647186257614,-13.55));
#31442=CARTESIAN_POINT('Ctrl Pts',(9.58129688507772,3.50147186257614,-9.58129688507772));
#31443=CARTESIAN_POINT('Ctrl Pts',(13.55,3.57647186257614,-5.61259377015545));
#31444=CARTESIAN_POINT('Ctrl Pts',(13.55,3.65147186257614,-2.489094619267E-15));
#31445=CARTESIAN_POINT('Ctrl Pts',(13.55,3.72647186257614,5.61259377015544));
#31446=CARTESIAN_POINT('Ctrl Pts',(9.58129688507772,3.80147186257614,9.58129688507772));
#31447=CARTESIAN_POINT('Ctrl Pts',(5.61259377015545,3.87647186257614,13.55));
#31448=CARTESIAN_POINT('Ctrl Pts',(0.,3.95147186257614,13.55));
#31449=CARTESIAN_POINT('Ctrl Pts',(-5.61259377015544,4.02647186257614,13.55));
#31450=CARTESIAN_POINT('Ctrl Pts',(-9.58129688507772,4.10147186257613,9.58129688507772));
#31451=CARTESIAN_POINT('Ctrl Pts',(-13.55,4.17647186257613,5.61259377015544));
#31452=CARTESIAN_POINT('Ctrl Pts',(-13.55,4.25147186257614,8.29698206422332E-16));
#31453=CARTESIAN_POINT('Ctrl Pts',(-13.55,4.32647186257613,-5.61259377015544));
#31454=CARTESIAN_POINT('Ctrl Pts',(-9.58129688507772,4.40147186257613,-9.58129688507772));
#31455=CARTESIAN_POINT('Ctrl Pts',(-5.61259377015544,4.47647186257614,-13.55));
#31456=CARTESIAN_POINT('Ctrl Pts',(-1.65939641284466E-15,4.55147186257613,
-13.55));
#31457=CARTESIAN_POINT('Ctrl Pts',(5.61259377015544,4.62647186257613,-13.55));
#31458=CARTESIAN_POINT('Ctrl Pts',(9.58129688507772,4.70147186257613,-9.58129688507772));
#31459=CARTESIAN_POINT('Ctrl Pts',(13.55,4.77647186257613,-5.61259377015545));
#31460=CARTESIAN_POINT('Ctrl Pts',(13.55,4.85147186257613,-2.489094619267E-15));
#31461=CARTESIAN_POINT('Ctrl Pts',(13.55,4.92647186257613,5.61259377015544));
#31462=CARTESIAN_POINT('Ctrl Pts',(9.58129688507772,5.00147186257613,9.58129688507772));
#31463=CARTESIAN_POINT('Ctrl Pts',(5.61259377015545,5.07647186257613,13.55));
#31464=CARTESIAN_POINT('Ctrl Pts',(0.,5.15147186257613,13.55));
#31465=CARTESIAN_POINT('Ctrl Pts',(0.,0.6,13.7985281374239));
#31466=CARTESIAN_POINT('Ctrl Pts',(-5.71553749530772,0.675,13.7985281374239));
#31467=CARTESIAN_POINT('Ctrl Pts',(-9.75703281636579,0.75,9.75703281636579));
#31468=CARTESIAN_POINT('Ctrl Pts',(-13.7985281374239,0.825,5.71553749530772));
#31469=CARTESIAN_POINT('Ctrl Pts',(-13.7985281374239,0.9,8.44916165822041E-16));
#31470=CARTESIAN_POINT('Ctrl Pts',(-13.7985281374239,0.974999999999999,
-5.71553749530772));
#31471=CARTESIAN_POINT('Ctrl Pts',(-9.75703281636579,1.05,-9.75703281636579));
#31472=CARTESIAN_POINT('Ctrl Pts',(-5.71553749530773,1.125,-13.7985281374239));
#31473=CARTESIAN_POINT('Ctrl Pts',(-1.68983233164408E-15,1.2,-13.7985281374239));
#31474=CARTESIAN_POINT('Ctrl Pts',(5.71553749530772,1.275,-13.7985281374239));
#31475=CARTESIAN_POINT('Ctrl Pts',(9.75703281636579,1.35,-9.75703281636579));
#31476=CARTESIAN_POINT('Ctrl Pts',(13.7985281374239,1.425,-5.71553749530773));
#31477=CARTESIAN_POINT('Ctrl Pts',(13.7985281374239,1.5,-2.53474849746612E-15));
#31478=CARTESIAN_POINT('Ctrl Pts',(13.7985281374239,1.575,5.71553749530773));
#31479=CARTESIAN_POINT('Ctrl Pts',(9.75703281636579,1.65,9.75703281636579));
#31480=CARTESIAN_POINT('Ctrl Pts',(5.71553749530774,1.725,13.7985281374239));
#31481=CARTESIAN_POINT('Ctrl Pts',(0.,1.8,13.7985281374239));
#31482=CARTESIAN_POINT('Ctrl Pts',(-5.71553749530772,1.875,13.7985281374239));
#31483=CARTESIAN_POINT('Ctrl Pts',(-9.75703281636579,1.95,9.75703281636579));
#31484=CARTESIAN_POINT('Ctrl Pts',(-13.7985281374239,2.025,5.71553749530772));
#31485=CARTESIAN_POINT('Ctrl Pts',(-13.7985281374239,2.1,8.44916165822041E-16));
#31486=CARTESIAN_POINT('Ctrl Pts',(-13.7985281374239,2.175,-5.71553749530772));
#31487=CARTESIAN_POINT('Ctrl Pts',(-9.75703281636579,2.25,-9.75703281636579));
#31488=CARTESIAN_POINT('Ctrl Pts',(-5.71553749530773,2.325,-13.7985281374239));
#31489=CARTESIAN_POINT('Ctrl Pts',(-1.68983233164408E-15,2.4,-13.7985281374239));
#31490=CARTESIAN_POINT('Ctrl Pts',(5.71553749530772,2.475,-13.7985281374239));
#31491=CARTESIAN_POINT('Ctrl Pts',(9.75703281636579,2.55,-9.75703281636579));
#31492=CARTESIAN_POINT('Ctrl Pts',(13.7985281374239,2.625,-5.71553749530773));
#31493=CARTESIAN_POINT('Ctrl Pts',(13.7985281374239,2.7,-2.53474849746612E-15));
#31494=CARTESIAN_POINT('Ctrl Pts',(13.7985281374239,2.775,5.71553749530773));
#31495=CARTESIAN_POINT('Ctrl Pts',(9.75703281636579,2.85,9.75703281636579));
#31496=CARTESIAN_POINT('Ctrl Pts',(5.71553749530774,2.92499999999999,13.7985281374239));
#31497=CARTESIAN_POINT('Ctrl Pts',(0.,2.99999999999999,13.7985281374239));
#31498=CARTESIAN_POINT('Ctrl Pts',(-5.71553749530772,3.075,13.7985281374239));
#31499=CARTESIAN_POINT('Ctrl Pts',(-9.75703281636579,3.14999999999999,9.75703281636579));
#31500=CARTESIAN_POINT('Ctrl Pts',(-13.7985281374239,3.22499999999999,5.71553749530772));
#31501=CARTESIAN_POINT('Ctrl Pts',(-13.7985281374239,3.29999999999999,8.44916165822041E-16));
#31502=CARTESIAN_POINT('Ctrl Pts',(-13.7985281374239,3.37499999999999,-5.71553749530772));
#31503=CARTESIAN_POINT('Ctrl Pts',(-9.75703281636579,3.44999999999999,-9.75703281636579));
#31504=CARTESIAN_POINT('Ctrl Pts',(-5.71553749530773,3.52499999999999,-13.7985281374239));
#31505=CARTESIAN_POINT('Ctrl Pts',(-1.68983233164408E-15,3.59999999999999,
-13.7985281374239));
#31506=CARTESIAN_POINT('Ctrl Pts',(5.71553749530772,3.67499999999999,-13.7985281374239));
#31507=CARTESIAN_POINT('Ctrl Pts',(9.75703281636579,3.74999999999999,-9.75703281636579));
#31508=CARTESIAN_POINT('Ctrl Pts',(13.7985281374239,3.82499999999999,-5.71553749530773));
#31509=CARTESIAN_POINT('Ctrl Pts',(13.7985281374239,3.89999999999999,-2.53474849746612E-15));
#31510=CARTESIAN_POINT('Ctrl Pts',(13.7985281374239,3.97499999999999,5.71553749530773));
#31511=CARTESIAN_POINT('Ctrl Pts',(9.75703281636579,4.04999999999999,9.75703281636579));
#31512=CARTESIAN_POINT('Ctrl Pts',(5.71553749530774,4.12499999999999,13.7985281374239));
#31513=CARTESIAN_POINT('Ctrl Pts',(0.,4.19999999999999,13.7985281374239));
#31514=CARTESIAN_POINT('Ctrl Pts',(-5.71553749530772,4.27499999999999,13.7985281374239));
#31515=CARTESIAN_POINT('Ctrl Pts',(-9.75703281636579,4.34999999999999,9.75703281636579));
#31516=CARTESIAN_POINT('Ctrl Pts',(-13.7985281374239,4.42499999999999,5.71553749530772));
#31517=CARTESIAN_POINT('Ctrl Pts',(-13.7985281374239,4.49999999999999,8.44916165822041E-16));
#31518=CARTESIAN_POINT('Ctrl Pts',(-13.7985281374239,4.57499999999999,-5.71553749530772));
#31519=CARTESIAN_POINT('Ctrl Pts',(-9.75703281636579,4.64999999999999,-9.75703281636579));
#31520=CARTESIAN_POINT('Ctrl Pts',(-5.71553749530773,4.72499999999999,-13.7985281374239));
#31521=CARTESIAN_POINT('Ctrl Pts',(-1.68983233164408E-15,4.79999999999999,
-13.7985281374239));
#31522=CARTESIAN_POINT('Ctrl Pts',(5.71553749530772,4.87499999999999,-13.7985281374239));
#31523=CARTESIAN_POINT('Ctrl Pts',(9.75703281636579,4.94999999999999,-9.75703281636579));
#31524=CARTESIAN_POINT('Ctrl Pts',(13.7985281374239,5.02499999999999,-5.71553749530773));
#31525=CARTESIAN_POINT('Ctrl Pts',(13.7985281374239,5.09999999999999,-2.53474849746612E-15));
#31526=CARTESIAN_POINT('Ctrl Pts',(13.7985281374239,5.17499999999999,5.71553749530773));
#31527=CARTESIAN_POINT('Ctrl Pts',(9.75703281636579,5.24999999999999,9.75703281636579));
#31528=CARTESIAN_POINT('Ctrl Pts',(5.71553749530774,5.32499999999999,13.7985281374239));
#31529=CARTESIAN_POINT('Ctrl Pts',(0.,5.39999999999999,13.7985281374239));
#31530=CARTESIAN_POINT('Ctrl Pts',(0.,0.6,14.15));
#31531=CARTESIAN_POINT('Ctrl Pts',(-5.8611219075793,0.675,14.15));
#31532=CARTESIAN_POINT('Ctrl Pts',(-10.0055609537896,0.75,10.0055609537896));
#31533=CARTESIAN_POINT('Ctrl Pts',(-14.15,0.825,5.8611219075793));
#31534=CARTESIAN_POINT('Ctrl Pts',(-14.15,0.9,8.66437610396752E-16));
#31535=CARTESIAN_POINT('Ctrl Pts',(-14.15,0.974999999999999,-5.86112190757929));
#31536=CARTESIAN_POINT('Ctrl Pts',(-10.0055609537896,1.05,-10.0055609537896));
#31537=CARTESIAN_POINT('Ctrl Pts',(-5.8611219075793,1.125,-14.15));
#31538=CARTESIAN_POINT('Ctrl Pts',(-1.7328752207935E-15,1.2,-14.15));
#31539=CARTESIAN_POINT('Ctrl Pts',(5.86112190757929,1.275,-14.15));
#31540=CARTESIAN_POINT('Ctrl Pts',(10.0055609537896,1.35,-10.0055609537896));
#31541=CARTESIAN_POINT('Ctrl Pts',(14.15,1.425,-5.8611219075793));
#31542=CARTESIAN_POINT('Ctrl Pts',(14.15,1.5,-2.59931283119026E-15));
#31543=CARTESIAN_POINT('Ctrl Pts',(14.15,1.575,5.8611219075793));
#31544=CARTESIAN_POINT('Ctrl Pts',(10.0055609537896,1.65,10.0055609537896));
#31545=CARTESIAN_POINT('Ctrl Pts',(5.8611219075793,1.725,14.15));
#31546=CARTESIAN_POINT('Ctrl Pts',(0.,1.8,14.15));
#31547=CARTESIAN_POINT('Ctrl Pts',(-5.8611219075793,1.875,14.15));
#31548=CARTESIAN_POINT('Ctrl Pts',(-10.0055609537896,1.95,10.0055609537896));
#31549=CARTESIAN_POINT('Ctrl Pts',(-14.15,2.025,5.8611219075793));
#31550=CARTESIAN_POINT('Ctrl Pts',(-14.15,2.1,8.66437610396752E-16));
#31551=CARTESIAN_POINT('Ctrl Pts',(-14.15,2.175,-5.86112190757929));
#31552=CARTESIAN_POINT('Ctrl Pts',(-10.0055609537896,2.25,-10.0055609537896));
#31553=CARTESIAN_POINT('Ctrl Pts',(-5.8611219075793,2.325,-14.15));
#31554=CARTESIAN_POINT('Ctrl Pts',(-1.7328752207935E-15,2.4,-14.15));
#31555=CARTESIAN_POINT('Ctrl Pts',(5.86112190757929,2.475,-14.15));
#31556=CARTESIAN_POINT('Ctrl Pts',(10.0055609537896,2.55,-10.0055609537896));
#31557=CARTESIAN_POINT('Ctrl Pts',(14.15,2.625,-5.8611219075793));
#31558=CARTESIAN_POINT('Ctrl Pts',(14.15,2.7,-2.59931283119026E-15));
#31559=CARTESIAN_POINT('Ctrl Pts',(14.15,2.775,5.8611219075793));
#31560=CARTESIAN_POINT('Ctrl Pts',(10.0055609537896,2.85,10.0055609537896));
#31561=CARTESIAN_POINT('Ctrl Pts',(5.8611219075793,2.92499999999999,14.15));
#31562=CARTESIAN_POINT('Ctrl Pts',(0.,2.99999999999999,14.15));
#31563=CARTESIAN_POINT('Ctrl Pts',(-5.8611219075793,3.07499999999999,14.15));
#31564=CARTESIAN_POINT('Ctrl Pts',(-10.0055609537896,3.15,10.0055609537896));
#31565=CARTESIAN_POINT('Ctrl Pts',(-14.15,3.22499999999999,5.8611219075793));
#31566=CARTESIAN_POINT('Ctrl Pts',(-14.15,3.29999999999999,8.66437610396752E-16));
#31567=CARTESIAN_POINT('Ctrl Pts',(-14.15,3.37499999999999,-5.86112190757929));
#31568=CARTESIAN_POINT('Ctrl Pts',(-10.0055609537896,3.44999999999999,-10.0055609537896));
#31569=CARTESIAN_POINT('Ctrl Pts',(-5.8611219075793,3.52499999999999,-14.15));
#31570=CARTESIAN_POINT('Ctrl Pts',(-1.7328752207935E-15,3.59999999999999,
-14.15));
#31571=CARTESIAN_POINT('Ctrl Pts',(5.86112190757929,3.67499999999999,-14.15));
#31572=CARTESIAN_POINT('Ctrl Pts',(10.0055609537896,3.74999999999999,-10.0055609537896));
#31573=CARTESIAN_POINT('Ctrl Pts',(14.15,3.82499999999999,-5.8611219075793));
#31574=CARTESIAN_POINT('Ctrl Pts',(14.15,3.89999999999999,-2.59931283119026E-15));
#31575=CARTESIAN_POINT('Ctrl Pts',(14.15,3.97499999999999,5.8611219075793));
#31576=CARTESIAN_POINT('Ctrl Pts',(10.0055609537896,4.04999999999999,10.0055609537896));
#31577=CARTESIAN_POINT('Ctrl Pts',(5.8611219075793,4.12499999999999,14.15));
#31578=CARTESIAN_POINT('Ctrl Pts',(0.,4.19999999999999,14.15));
#31579=CARTESIAN_POINT('Ctrl Pts',(-5.8611219075793,4.27499999999999,14.15));
#31580=CARTESIAN_POINT('Ctrl Pts',(-10.0055609537896,4.34999999999999,10.0055609537896));
#31581=CARTESIAN_POINT('Ctrl Pts',(-14.15,4.42499999999999,5.8611219075793));
#31582=CARTESIAN_POINT('Ctrl Pts',(-14.15,4.49999999999999,8.66437610396752E-16));
#31583=CARTESIAN_POINT('Ctrl Pts',(-14.15,4.57499999999999,-5.86112190757929));
#31584=CARTESIAN_POINT('Ctrl Pts',(-10.0055609537896,4.64999999999999,-10.0055609537896));
#31585=CARTESIAN_POINT('Ctrl Pts',(-5.8611219075793,4.72499999999999,-14.15));
#31586=CARTESIAN_POINT('Ctrl Pts',(-1.7328752207935E-15,4.79999999999999,
-14.15));
#31587=CARTESIAN_POINT('Ctrl Pts',(5.86112190757929,4.87499999999999,-14.15));
#31588=CARTESIAN_POINT('Ctrl Pts',(10.0055609537896,4.94999999999999,-10.0055609537896));
#31589=CARTESIAN_POINT('Ctrl Pts',(14.15,5.02499999999999,-5.8611219075793));
#31590=CARTESIAN_POINT('Ctrl Pts',(14.15,5.09999999999999,-2.59931283119026E-15));
#31591=CARTESIAN_POINT('Ctrl Pts',(14.15,5.17499999999999,5.8611219075793));
#31592=CARTESIAN_POINT('Ctrl Pts',(10.0055609537896,5.24999999999999,10.0055609537896));
#31593=CARTESIAN_POINT('Ctrl Pts',(5.8611219075793,5.32499999999999,14.15));
#31594=CARTESIAN_POINT('Ctrl Pts',(0.,5.39999999999999,14.15));
#31595=CARTESIAN_POINT('',(-3.71838991479217E-13,4.79999999999999,13.55));
#31596=CARTESIAN_POINT('',(-3.86571311453075E-13,5.39999999999999,14.15));
#31597=CARTESIAN_POINT('Origin',(-7.90471375114085E-13,4.8,14.15));
#31598=CARTESIAN_POINT('',(-3.90037061894662E-13,4.2,14.15));
#31599=CARTESIAN_POINT('Ctrl Pts',(1.21301265455545E-14,4.19999999999999,
14.15));
#31600=CARTESIAN_POINT('Ctrl Pts',(-5.86112190757927,4.27499999999999,14.15));
#31601=CARTESIAN_POINT('Ctrl Pts',(-10.0055609537896,4.34999999999999,10.0055609537896));
#31602=CARTESIAN_POINT('Ctrl Pts',(-14.15,4.42499999999999,5.86112190757931));
#31603=CARTESIAN_POINT('Ctrl Pts',(-14.15,4.49999999999999,-1.21388851215623E-14));
#31604=CARTESIAN_POINT('Ctrl Pts',(-14.15,4.57499999999999,-5.86112190757929));
#31605=CARTESIAN_POINT('Ctrl Pts',(-10.0055609537897,4.64999999999999,-10.0055609537896));
#31606=CARTESIAN_POINT('Ctrl Pts',(-5.86112190757929,4.72499999999999,-14.15));
#31607=CARTESIAN_POINT('Ctrl Pts',(-1.3863001766348E-14,4.79999999999999,
-14.15));
#31608=CARTESIAN_POINT('Ctrl Pts',(5.86112190757926,4.87499999999999,-14.15));
#31609=CARTESIAN_POINT('Ctrl Pts',(10.0055609537896,4.94999999999999,-10.0055609537896));
#31610=CARTESIAN_POINT('Ctrl Pts',(14.15,5.02499999999999,-5.86112190757932));
#31611=CARTESIAN_POINT('Ctrl Pts',(14.15,5.09999999999999,-3.98648886542583E-14));
#31612=CARTESIAN_POINT('Ctrl Pts',(14.15,5.17499999999999,5.86112190757929));
#31613=CARTESIAN_POINT('Ctrl Pts',(10.0055609537897,5.24999999999999,10.0055609537896));
#31614=CARTESIAN_POINT('Ctrl Pts',(5.86112190757929,5.32499999999999,14.15));
#31615=CARTESIAN_POINT('Ctrl Pts',(-3.86571311453075E-13,5.39999999999999,
14.15));
#31616=CARTESIAN_POINT('',(1.7328752207935E-15,0.599999999999999,14.15));
#31617=CARTESIAN_POINT('Ctrl Pts',(1.7328752207935E-15,0.599999999999999,
14.15));
#31618=CARTESIAN_POINT('Ctrl Pts',(-5.86112190757929,0.674999999999999,
14.15));
#31619=CARTESIAN_POINT('Ctrl Pts',(-10.0055609537896,0.749999999999998,
10.0055609537896));
#31620=CARTESIAN_POINT('Ctrl Pts',(-14.15,0.824999999999999,5.8611219075793));
#31621=CARTESIAN_POINT('Ctrl Pts',(-14.15,0.899999999999998,2.59931283119026E-15));
#31622=CARTESIAN_POINT('Ctrl Pts',(-14.15,0.974999999999998,-5.86112190757929));
#31623=CARTESIAN_POINT('Ctrl Pts',(-10.0055609537896,1.05,-10.0055609537896));
#31624=CARTESIAN_POINT('Ctrl Pts',(-5.8611219075793,1.125,-14.15));
#31625=CARTESIAN_POINT('Ctrl Pts',(-3.46575044158701E-15,1.2,-14.15));
#31626=CARTESIAN_POINT('Ctrl Pts',(5.86112190757929,1.275,-14.15));
#31627=CARTESIAN_POINT('Ctrl Pts',(10.0055609537896,1.35,-10.0055609537897));
#31628=CARTESIAN_POINT('Ctrl Pts',(14.15,1.425,-5.8611219075793));
#31629=CARTESIAN_POINT('Ctrl Pts',(14.15,1.5,-4.33218805198376E-15));
#31630=CARTESIAN_POINT('Ctrl Pts',(14.15,1.575,5.8611219075793));
#31631=CARTESIAN_POINT('Ctrl Pts',(10.0055609537897,1.65,10.0055609537896));
#31632=CARTESIAN_POINT('Ctrl Pts',(5.86112190757931,1.725,14.15));
#31633=CARTESIAN_POINT('Ctrl Pts',(5.19862566238051E-15,1.8,14.15));
#31634=CARTESIAN_POINT('Ctrl Pts',(-5.8611219075793,1.875,14.15));
#31635=CARTESIAN_POINT('Ctrl Pts',(-10.0055609537896,1.95,10.0055609537897));
#31636=CARTESIAN_POINT('Ctrl Pts',(-14.15,2.025,5.86112190757931));
#31637=CARTESIAN_POINT('Ctrl Pts',(-14.15,2.1,6.06506327277727E-15));
#31638=CARTESIAN_POINT('Ctrl Pts',(-14.15,2.175,-5.8611219075793));
#31639=CARTESIAN_POINT('Ctrl Pts',(-10.0055609537897,2.25,-10.0055609537896));
#31640=CARTESIAN_POINT('Ctrl Pts',(-5.86112190757931,2.32499999999999,-14.15));
#31641=CARTESIAN_POINT('Ctrl Pts',(-6.93150088317402E-15,2.4,-14.15));
#31642=CARTESIAN_POINT('Ctrl Pts',(5.86112190757929,2.475,-14.15));
#31643=CARTESIAN_POINT('Ctrl Pts',(10.0055609537896,2.54999999999999,-10.0055609537896));
#31644=CARTESIAN_POINT('Ctrl Pts',(14.15,2.625,-5.86112190757931));
#31645=CARTESIAN_POINT('Ctrl Pts',(14.15,2.69999999999999,-7.79793849357077E-15));
#31646=CARTESIAN_POINT('Ctrl Pts',(14.15,2.77499999999999,5.86112190757929));
#31647=CARTESIAN_POINT('Ctrl Pts',(10.0055609537897,2.84999999999999,10.0055609537896));
#31648=CARTESIAN_POINT('Ctrl Pts',(5.86112190757931,2.92499999999999,14.15));
#31649=CARTESIAN_POINT('Ctrl Pts',(8.66437610396752E-15,2.99999999999999,
14.15));
#31650=CARTESIAN_POINT('Ctrl Pts',(-5.86112190757929,3.07499999999999,14.15));
#31651=CARTESIAN_POINT('Ctrl Pts',(-10.0055609537896,3.14999999999999,10.0055609537896));
#31652=CARTESIAN_POINT('Ctrl Pts',(-14.15,3.22499999999999,5.86112190757931));
#31653=CARTESIAN_POINT('Ctrl Pts',(-14.15,3.29999999999999,9.53081371436428E-15));
#31654=CARTESIAN_POINT('Ctrl Pts',(-14.15,3.37499999999999,-5.86112190757929));
#31655=CARTESIAN_POINT('Ctrl Pts',(-10.0055609537897,3.44999999999999,-10.0055609537896));
#31656=CARTESIAN_POINT('Ctrl Pts',(-5.86112190757931,3.52499999999999,-14.15));
#31657=CARTESIAN_POINT('Ctrl Pts',(-1.0397251324761E-14,3.59999999999999,
-14.15));
#31658=CARTESIAN_POINT('Ctrl Pts',(5.86112190757927,3.67499999999999,-14.15));
#31659=CARTESIAN_POINT('Ctrl Pts',(10.0055609537896,3.74999999999999,-10.0055609537896));
#31660=CARTESIAN_POINT('Ctrl Pts',(14.15,3.82499999999999,-5.86112190757931));
#31661=CARTESIAN_POINT('Ctrl Pts',(14.15,3.89999999999999,-3.63991382126713E-14));
#31662=CARTESIAN_POINT('Ctrl Pts',(14.15,3.97499999999999,5.86112190757929));
#31663=CARTESIAN_POINT('Ctrl Pts',(10.0055609537897,4.04999999999999,10.0055609537896));
#31664=CARTESIAN_POINT('Ctrl Pts',(5.86112190757929,4.12499999999999,14.15));
#31665=CARTESIAN_POINT('Ctrl Pts',(1.21301265455545E-14,4.19999999999999,
14.15));
#31666=CARTESIAN_POINT('',(0.,0.,13.55));
#31667=CARTESIAN_POINT('Origin',(0.,0.,14.15));
#31668=CARTESIAN_POINT('Ctrl Pts',(0.,0.,13.55));
#31669=CARTESIAN_POINT('Ctrl Pts',(-5.61259377015544,0.0749999999999999,
13.55));
#31670=CARTESIAN_POINT('Ctrl Pts',(-9.58129688507772,0.15,9.58129688507772));
#31671=CARTESIAN_POINT('Ctrl Pts',(-13.55,0.225,5.61259377015544));
#31672=CARTESIAN_POINT('Ctrl Pts',(-13.55,0.299999999999999,8.29698206422332E-16));
#31673=CARTESIAN_POINT('Ctrl Pts',(-13.55,0.374999999999999,-5.61259377015544));
#31674=CARTESIAN_POINT('Ctrl Pts',(-9.58129688507772,0.449999999999999,
-9.58129688507772));
#31675=CARTESIAN_POINT('Ctrl Pts',(-5.61259377015544,0.524999999999999,
-13.55));
#31676=CARTESIAN_POINT('Ctrl Pts',(-1.65939641284466E-15,0.599999999999999,
-13.55));
#31677=CARTESIAN_POINT('Ctrl Pts',(5.61259377015544,0.674999999999998,-13.55));
#31678=CARTESIAN_POINT('Ctrl Pts',(9.58129688507772,0.749999999999998,-9.58129688507772));
#31679=CARTESIAN_POINT('Ctrl Pts',(13.55,0.824999999999998,-5.61259377015545));
#31680=CARTESIAN_POINT('Ctrl Pts',(13.55,0.899999999999998,-2.489094619267E-15));
#31681=CARTESIAN_POINT('Ctrl Pts',(13.55,0.974999999999998,5.61259377015544));
#31682=CARTESIAN_POINT('Ctrl Pts',(9.58129688507772,1.05,9.58129688507772));
#31683=CARTESIAN_POINT('Ctrl Pts',(5.61259377015545,1.125,13.55));
#31684=CARTESIAN_POINT('Ctrl Pts',(3.31879282568933E-15,1.2,13.55));
#31685=CARTESIAN_POINT('Ctrl Pts',(-5.61259377015544,1.275,13.55));
#31686=CARTESIAN_POINT('Ctrl Pts',(-9.58129688507772,1.35,9.58129688507772));
#31687=CARTESIAN_POINT('Ctrl Pts',(-13.55,1.425,5.61259377015545));
#31688=CARTESIAN_POINT('Ctrl Pts',(-13.55,1.5,4.14849103211166E-15));
#31689=CARTESIAN_POINT('Ctrl Pts',(-13.55,1.575,-5.61259377015544));
#31690=CARTESIAN_POINT('Ctrl Pts',(-9.58129688507773,1.65,-9.58129688507771));
#31691=CARTESIAN_POINT('Ctrl Pts',(-5.61259377015545,1.725,-13.55));
#31692=CARTESIAN_POINT('Ctrl Pts',(-4.97818923853399E-15,1.8,-13.55));
#31693=CARTESIAN_POINT('Ctrl Pts',(5.61259377015544,1.875,-13.55));
#31694=CARTESIAN_POINT('Ctrl Pts',(9.58129688507773,1.95,-9.58129688507771));
#31695=CARTESIAN_POINT('Ctrl Pts',(13.55,2.025,-5.61259377015545));
#31696=CARTESIAN_POINT('Ctrl Pts',(13.55,2.1,-5.80788744495632E-15));
#31697=CARTESIAN_POINT('Ctrl Pts',(13.55,2.17499999999999,5.61259377015544));
#31698=CARTESIAN_POINT('Ctrl Pts',(9.58129688507773,2.25,9.58129688507771));
#31699=CARTESIAN_POINT('Ctrl Pts',(5.61259377015545,2.32499999999999,13.55));
#31700=CARTESIAN_POINT('Ctrl Pts',(6.63758565137865E-15,2.39999999999999,
13.55));
#31701=CARTESIAN_POINT('Ctrl Pts',(-5.61259377015544,2.475,13.55));
#31702=CARTESIAN_POINT('Ctrl Pts',(-9.58129688507772,2.54999999999999,9.58129688507772));
#31703=CARTESIAN_POINT('Ctrl Pts',(-13.55,2.62499999999999,5.61259377015545));
#31704=CARTESIAN_POINT('Ctrl Pts',(-13.55,2.69999999999999,7.46728385780099E-15));
#31705=CARTESIAN_POINT('Ctrl Pts',(-13.55,2.77499999999999,-5.61259377015544));
#31706=CARTESIAN_POINT('Ctrl Pts',(-9.58129688507773,2.84999999999999,-9.5812968850777));
#31707=CARTESIAN_POINT('Ctrl Pts',(-5.61259377015545,2.92499999999999,-13.55));
#31708=CARTESIAN_POINT('Ctrl Pts',(-8.29698206422332E-15,2.99999999999999,
-13.55));
#31709=CARTESIAN_POINT('Ctrl Pts',(5.61259377015541,3.07499999999999,-13.55));
#31710=CARTESIAN_POINT('Ctrl Pts',(9.58129688507772,3.14999999999999,-9.58129688507772));
#31711=CARTESIAN_POINT('Ctrl Pts',(13.55,3.22499999999999,-5.61259377015545));
#31712=CARTESIAN_POINT('Ctrl Pts',(13.55,3.29999999999999,-3.3196315444519E-14));
#31713=CARTESIAN_POINT('Ctrl Pts',(13.55,3.37499999999999,5.61259377015544));
#31714=CARTESIAN_POINT('Ctrl Pts',(9.58129688507773,3.44999999999999,9.5812968850777));
#31715=CARTESIAN_POINT('Ctrl Pts',(5.61259377015543,3.52499999999999,13.55));
#31716=CARTESIAN_POINT('Ctrl Pts',(9.95637847706798E-15,3.59999999999999,
13.55));
#31717=CARTESIAN_POINT('Ctrl Pts',(-5.61259377015541,3.67499999999999,13.55));
#31718=CARTESIAN_POINT('Ctrl Pts',(-9.58129688507772,3.74999999999999,9.58129688507772));
#31719=CARTESIAN_POINT('Ctrl Pts',(-13.55,3.82499999999999,5.61259377015546));
#31720=CARTESIAN_POINT('Ctrl Pts',(-13.55,3.89999999999999,-1.32835584903831E-14));
#31721=CARTESIAN_POINT('Ctrl Pts',(-13.55,3.97499999999999,-5.61259377015543));
#31722=CARTESIAN_POINT('Ctrl Pts',(-9.58129688507774,4.04999999999999,-9.5812968850777));
#31723=CARTESIAN_POINT('Ctrl Pts',(-5.61259377015543,4.12499999999999,-13.55));
#31724=CARTESIAN_POINT('Ctrl Pts',(-1.16157748899126E-14,4.19999999999999,
-13.55));
#31725=CARTESIAN_POINT('Ctrl Pts',(5.61259377015541,4.27499999999999,-13.55));
#31726=CARTESIAN_POINT('Ctrl Pts',(9.58129688507772,4.34999999999999,-9.58129688507772));
#31727=CARTESIAN_POINT('Ctrl Pts',(13.55,4.42499999999999,-5.61259377015546));
#31728=CARTESIAN_POINT('Ctrl Pts',(13.55,4.49999999999999,-3.65151082702084E-14));
#31729=CARTESIAN_POINT('Ctrl Pts',(13.55,4.57499999999999,5.61259377015543));
#31730=CARTESIAN_POINT('Ctrl Pts',(9.58129688507774,4.64999999999999,9.5812968850777));
#31731=CARTESIAN_POINT('Ctrl Pts',(5.61259377015543,4.72499999999999,13.55));
#31732=CARTESIAN_POINT('Ctrl Pts',(-3.71838991479217E-13,4.79999999999999,
13.55));
#31733=CARTESIAN_POINT('Ctrl Pts',(0.,-0.6,14.15));
#31734=CARTESIAN_POINT('Ctrl Pts',(-5.8611219075793,-0.525,14.15));
#31735=CARTESIAN_POINT('Ctrl Pts',(-10.0055609537896,-0.450000000000001,
10.0055609537896));
#31736=CARTESIAN_POINT('Ctrl Pts',(-14.15,-0.375000000000001,5.8611219075793));
#31737=CARTESIAN_POINT('Ctrl Pts',(-14.15,-0.300000000000001,8.66437610396752E-16));
#31738=CARTESIAN_POINT('Ctrl Pts',(-14.15,-0.225000000000001,-5.86112190757929));
#31739=CARTESIAN_POINT('Ctrl Pts',(-10.0055609537896,-0.150000000000001,
-10.0055609537896));
#31740=CARTESIAN_POINT('Ctrl Pts',(-5.8611219075793,-0.0750000000000014,
-14.15));
#31741=CARTESIAN_POINT('Ctrl Pts',(-1.7328752207935E-15,-1.51788304147971E-15,
-14.15));
#31742=CARTESIAN_POINT('Ctrl Pts',(5.86112190757929,0.0749999999999984,
-14.15));
#31743=CARTESIAN_POINT('Ctrl Pts',(10.0055609537896,0.149999999999998,-10.0055609537896));
#31744=CARTESIAN_POINT('Ctrl Pts',(14.15,0.224999999999998,-5.8611219075793));
#31745=CARTESIAN_POINT('Ctrl Pts',(14.15,0.299999999999998,-2.59931283119026E-15));
#31746=CARTESIAN_POINT('Ctrl Pts',(14.15,0.374999999999998,5.8611219075793));
#31747=CARTESIAN_POINT('Ctrl Pts',(10.0055609537896,0.449999999999997,10.0055609537896));
#31748=CARTESIAN_POINT('Ctrl Pts',(5.8611219075793,0.524999999999997,14.15));
#31749=CARTESIAN_POINT('Ctrl Pts',(0.,0.599999999999997,14.15));
#31750=CARTESIAN_POINT('Ctrl Pts',(-5.8611219075793,0.674999999999997,14.15));
#31751=CARTESIAN_POINT('Ctrl Pts',(-10.0055609537896,0.749999999999997,
10.0055609537896));
#31752=CARTESIAN_POINT('Ctrl Pts',(-14.15,0.824999999999997,5.8611219075793));
#31753=CARTESIAN_POINT('Ctrl Pts',(-14.15,0.899999999999996,8.66437610396752E-16));
#31754=CARTESIAN_POINT('Ctrl Pts',(-14.15,0.974999999999996,-5.86112190757929));
#31755=CARTESIAN_POINT('Ctrl Pts',(-10.0055609537896,1.05,-10.0055609537896));
#31756=CARTESIAN_POINT('Ctrl Pts',(-5.8611219075793,1.125,-14.15));
#31757=CARTESIAN_POINT('Ctrl Pts',(-1.7328752207935E-15,1.2,-14.15));
#31758=CARTESIAN_POINT('Ctrl Pts',(5.86112190757929,1.275,-14.15));
#31759=CARTESIAN_POINT('Ctrl Pts',(10.0055609537896,1.35,-10.0055609537896));
#31760=CARTESIAN_POINT('Ctrl Pts',(14.15,1.425,-5.8611219075793));
#31761=CARTESIAN_POINT('Ctrl Pts',(14.15,1.49999999999999,-2.59931283119026E-15));
#31762=CARTESIAN_POINT('Ctrl Pts',(14.15,1.57499999999999,5.8611219075793));
#31763=CARTESIAN_POINT('Ctrl Pts',(10.0055609537896,1.64999999999999,10.0055609537896));
#31764=CARTESIAN_POINT('Ctrl Pts',(5.8611219075793,1.72499999999999,14.15));
#31765=CARTESIAN_POINT('Ctrl Pts',(0.,1.79999999999999,14.15));
#31766=CARTESIAN_POINT('Ctrl Pts',(-5.8611219075793,1.87499999999999,14.15));
#31767=CARTESIAN_POINT('Ctrl Pts',(-10.0055609537896,1.94999999999999,10.0055609537896));
#31768=CARTESIAN_POINT('Ctrl Pts',(-14.15,2.02499999999999,5.8611219075793));
#31769=CARTESIAN_POINT('Ctrl Pts',(-14.15,2.09999999999999,8.66437610396752E-16));
#31770=CARTESIAN_POINT('Ctrl Pts',(-14.15,2.17499999999999,-5.86112190757929));
#31771=CARTESIAN_POINT('Ctrl Pts',(-10.0055609537896,2.24999999999999,-10.0055609537896));
#31772=CARTESIAN_POINT('Ctrl Pts',(-5.8611219075793,2.32499999999999,-14.15));
#31773=CARTESIAN_POINT('Ctrl Pts',(-1.7328752207935E-15,2.39999999999999,
-14.15));
#31774=CARTESIAN_POINT('Ctrl Pts',(5.86112190757929,2.47499999999999,-14.15));
#31775=CARTESIAN_POINT('Ctrl Pts',(10.0055609537896,2.54999999999999,-10.0055609537896));
#31776=CARTESIAN_POINT('Ctrl Pts',(14.15,2.62499999999999,-5.8611219075793));
#31777=CARTESIAN_POINT('Ctrl Pts',(14.15,2.69999999999999,-2.59931283119026E-15));
#31778=CARTESIAN_POINT('Ctrl Pts',(14.15,2.77499999999999,5.8611219075793));
#31779=CARTESIAN_POINT('Ctrl Pts',(10.0055609537896,2.84999999999999,10.0055609537896));
#31780=CARTESIAN_POINT('Ctrl Pts',(5.8611219075793,2.92499999999999,14.15));
#31781=CARTESIAN_POINT('Ctrl Pts',(0.,2.99999999999999,14.15));
#31782=CARTESIAN_POINT('Ctrl Pts',(-5.8611219075793,3.07499999999999,14.15));
#31783=CARTESIAN_POINT('Ctrl Pts',(-10.0055609537896,3.14999999999999,10.0055609537896));
#31784=CARTESIAN_POINT('Ctrl Pts',(-14.15,3.22499999999999,5.8611219075793));
#31785=CARTESIAN_POINT('Ctrl Pts',(-14.15,3.29999999999999,8.66437610396752E-16));
#31786=CARTESIAN_POINT('Ctrl Pts',(-14.15,3.37499999999999,-5.86112190757929));
#31787=CARTESIAN_POINT('Ctrl Pts',(-10.0055609537896,3.44999999999999,-10.0055609537896));
#31788=CARTESIAN_POINT('Ctrl Pts',(-5.8611219075793,3.52499999999999,-14.15));
#31789=CARTESIAN_POINT('Ctrl Pts',(-1.7328752207935E-15,3.59999999999999,
-14.15));
#31790=CARTESIAN_POINT('Ctrl Pts',(5.86112190757929,3.67499999999999,-14.15));
#31791=CARTESIAN_POINT('Ctrl Pts',(10.0055609537896,3.74999999999999,-10.0055609537896));
#31792=CARTESIAN_POINT('Ctrl Pts',(14.15,3.82499999999999,-5.8611219075793));
#31793=CARTESIAN_POINT('Ctrl Pts',(14.15,3.89999999999999,-2.59931283119026E-15));
#31794=CARTESIAN_POINT('Ctrl Pts',(14.15,3.97499999999999,5.8611219075793));
#31795=CARTESIAN_POINT('Ctrl Pts',(10.0055609537896,4.04999999999999,10.0055609537896));
#31796=CARTESIAN_POINT('Ctrl Pts',(5.8611219075793,4.12499999999999,14.15));
#31797=CARTESIAN_POINT('Ctrl Pts',(0.,4.19999999999999,14.15));
#31798=CARTESIAN_POINT('Ctrl Pts',(0.,-0.6,13.7985281374239));
#31799=CARTESIAN_POINT('Ctrl Pts',(-5.71553749530772,-0.525,13.7985281374239));
#31800=CARTESIAN_POINT('Ctrl Pts',(-9.75703281636579,-0.450000000000001,
9.75703281636579));
#31801=CARTESIAN_POINT('Ctrl Pts',(-13.7985281374239,-0.375000000000001,
5.71553749530772));
#31802=CARTESIAN_POINT('Ctrl Pts',(-13.7985281374239,-0.300000000000001,
8.44916165822041E-16));
#31803=CARTESIAN_POINT('Ctrl Pts',(-13.7985281374239,-0.225000000000001,
-5.71553749530772));
#31804=CARTESIAN_POINT('Ctrl Pts',(-9.75703281636579,-0.150000000000001,
-9.75703281636579));
#31805=CARTESIAN_POINT('Ctrl Pts',(-5.71553749530773,-0.0750000000000015,
-13.7985281374239));
#31806=CARTESIAN_POINT('Ctrl Pts',(-1.68983233164408E-15,-1.62630325872826E-15,
-13.7985281374239));
#31807=CARTESIAN_POINT('Ctrl Pts',(5.71553749530772,0.0749999999999982,
-13.7985281374239));
#31808=CARTESIAN_POINT('Ctrl Pts',(9.75703281636579,0.149999999999998,-9.75703281636579));
#31809=CARTESIAN_POINT('Ctrl Pts',(13.7985281374239,0.224999999999998,-5.71553749530773));
#31810=CARTESIAN_POINT('Ctrl Pts',(13.7985281374239,0.299999999999998,-2.53474849746612E-15));
#31811=CARTESIAN_POINT('Ctrl Pts',(13.7985281374239,0.374999999999998,5.71553749530773));
#31812=CARTESIAN_POINT('Ctrl Pts',(9.75703281636579,0.449999999999997,9.75703281636579));
#31813=CARTESIAN_POINT('Ctrl Pts',(5.71553749530774,0.524999999999997,13.7985281374239));
#31814=CARTESIAN_POINT('Ctrl Pts',(0.,0.599999999999997,13.7985281374239));
#31815=CARTESIAN_POINT('Ctrl Pts',(-5.71553749530772,0.674999999999997,
13.7985281374239));
#31816=CARTESIAN_POINT('Ctrl Pts',(-9.75703281636579,0.749999999999997,
9.75703281636579));
#31817=CARTESIAN_POINT('Ctrl Pts',(-13.7985281374239,0.824999999999997,
5.71553749530772));
#31818=CARTESIAN_POINT('Ctrl Pts',(-13.7985281374239,0.899999999999996,
8.44916165822041E-16));
#31819=CARTESIAN_POINT('Ctrl Pts',(-13.7985281374239,0.974999999999996,
-5.71553749530772));
#31820=CARTESIAN_POINT('Ctrl Pts',(-9.75703281636579,1.05,-9.75703281636579));
#31821=CARTESIAN_POINT('Ctrl Pts',(-5.71553749530773,1.125,-13.7985281374239));
#31822=CARTESIAN_POINT('Ctrl Pts',(-1.68983233164408E-15,1.2,-13.7985281374239));
#31823=CARTESIAN_POINT('Ctrl Pts',(5.71553749530772,1.275,-13.7985281374239));
#31824=CARTESIAN_POINT('Ctrl Pts',(9.75703281636579,1.35,-9.75703281636579));
#31825=CARTESIAN_POINT('Ctrl Pts',(13.7985281374239,1.425,-5.71553749530773));
#31826=CARTESIAN_POINT('Ctrl Pts',(13.7985281374239,1.49999999999999,-2.53474849746612E-15));
#31827=CARTESIAN_POINT('Ctrl Pts',(13.7985281374239,1.57499999999999,5.71553749530773));
#31828=CARTESIAN_POINT('Ctrl Pts',(9.75703281636579,1.65,9.75703281636579));
#31829=CARTESIAN_POINT('Ctrl Pts',(5.71553749530774,1.72499999999999,13.7985281374239));
#31830=CARTESIAN_POINT('Ctrl Pts',(0.,1.79999999999999,13.7985281374239));
#31831=CARTESIAN_POINT('Ctrl Pts',(-5.71553749530772,1.87499999999999,13.7985281374239));
#31832=CARTESIAN_POINT('Ctrl Pts',(-9.75703281636579,1.94999999999999,9.75703281636579));
#31833=CARTESIAN_POINT('Ctrl Pts',(-13.7985281374239,2.02499999999999,5.71553749530772));
#31834=CARTESIAN_POINT('Ctrl Pts',(-13.7985281374239,2.09999999999999,8.44916165822041E-16));
#31835=CARTESIAN_POINT('Ctrl Pts',(-13.7985281374239,2.17499999999999,-5.71553749530772));
#31836=CARTESIAN_POINT('Ctrl Pts',(-9.75703281636579,2.24999999999999,-9.75703281636579));
#31837=CARTESIAN_POINT('Ctrl Pts',(-5.71553749530773,2.32499999999999,-13.7985281374239));
#31838=CARTESIAN_POINT('Ctrl Pts',(-1.68983233164408E-15,2.39999999999999,
-13.7985281374239));
#31839=CARTESIAN_POINT('Ctrl Pts',(5.71553749530772,2.47499999999999,-13.7985281374239));
#31840=CARTESIAN_POINT('Ctrl Pts',(9.75703281636579,2.54999999999999,-9.75703281636579));
#31841=CARTESIAN_POINT('Ctrl Pts',(13.7985281374239,2.62499999999999,-5.71553749530773));
#31842=CARTESIAN_POINT('Ctrl Pts',(13.7985281374239,2.69999999999999,-2.53474849746612E-15));
#31843=CARTESIAN_POINT('Ctrl Pts',(13.7985281374239,2.77499999999999,5.71553749530773));
#31844=CARTESIAN_POINT('Ctrl Pts',(9.75703281636579,2.84999999999999,9.75703281636579));
#31845=CARTESIAN_POINT('Ctrl Pts',(5.71553749530774,2.92499999999999,13.7985281374239));
#31846=CARTESIAN_POINT('Ctrl Pts',(0.,2.99999999999999,13.7985281374239));
#31847=CARTESIAN_POINT('Ctrl Pts',(-5.71553749530772,3.07499999999999,13.7985281374239));
#31848=CARTESIAN_POINT('Ctrl Pts',(-9.75703281636579,3.14999999999999,9.75703281636579));
#31849=CARTESIAN_POINT('Ctrl Pts',(-13.7985281374239,3.22499999999999,5.71553749530772));
#31850=CARTESIAN_POINT('Ctrl Pts',(-13.7985281374239,3.29999999999999,8.44916165822041E-16));
#31851=CARTESIAN_POINT('Ctrl Pts',(-13.7985281374239,3.37499999999999,-5.71553749530772));
#31852=CARTESIAN_POINT('Ctrl Pts',(-9.75703281636579,3.44999999999999,-9.75703281636579));
#31853=CARTESIAN_POINT('Ctrl Pts',(-5.71553749530773,3.52499999999999,-13.7985281374239));
#31854=CARTESIAN_POINT('Ctrl Pts',(-1.68983233164408E-15,3.59999999999999,
-13.7985281374239));
#31855=CARTESIAN_POINT('Ctrl Pts',(5.71553749530772,3.67499999999999,-13.7985281374239));
#31856=CARTESIAN_POINT('Ctrl Pts',(9.75703281636579,3.74999999999999,-9.75703281636579));
#31857=CARTESIAN_POINT('Ctrl Pts',(13.7985281374239,3.82499999999999,-5.71553749530773));
#31858=CARTESIAN_POINT('Ctrl Pts',(13.7985281374239,3.89999999999999,-2.53474849746612E-15));
#31859=CARTESIAN_POINT('Ctrl Pts',(13.7985281374239,3.97499999999999,5.71553749530773));
#31860=CARTESIAN_POINT('Ctrl Pts',(9.75703281636579,4.04999999999999,9.75703281636579));
#31861=CARTESIAN_POINT('Ctrl Pts',(5.71553749530774,4.12499999999999,13.7985281374239));
#31862=CARTESIAN_POINT('Ctrl Pts',(0.,4.19999999999999,13.7985281374239));
#31863=CARTESIAN_POINT('Ctrl Pts',(0.,-0.351471862576143,13.55));
#31864=CARTESIAN_POINT('Ctrl Pts',(-5.61259377015544,-0.276471862576143,
13.55));
#31865=CARTESIAN_POINT('Ctrl Pts',(-9.58129688507772,-0.201471862576143,
9.58129688507772));
#31866=CARTESIAN_POINT('Ctrl Pts',(-13.55,-0.126471862576144,5.61259377015544));
#31867=CARTESIAN_POINT('Ctrl Pts',(-13.55,-0.0514718625761438,8.29698206422332E-16));
#31868=CARTESIAN_POINT('Ctrl Pts',(-13.55,0.0235281374238561,-5.61259377015544));
#31869=CARTESIAN_POINT('Ctrl Pts',(-9.58129688507772,0.098528137423856,
-9.58129688507772));
#31870=CARTESIAN_POINT('Ctrl Pts',(-5.61259377015544,0.173528137423856,
-13.55));
#31871=CARTESIAN_POINT('Ctrl Pts',(-1.65939641284466E-15,0.248528137423856,
-13.55));
#31872=CARTESIAN_POINT('Ctrl Pts',(5.61259377015544,0.323528137423855,-13.55));
#31873=CARTESIAN_POINT('Ctrl Pts',(9.58129688507772,0.398528137423855,-9.58129688507772));
#31874=CARTESIAN_POINT('Ctrl Pts',(13.55,0.473528137423855,-5.61259377015545));
#31875=CARTESIAN_POINT('Ctrl Pts',(13.55,0.548528137423855,-2.489094619267E-15));
#31876=CARTESIAN_POINT('Ctrl Pts',(13.55,0.623528137423855,5.61259377015544));
#31877=CARTESIAN_POINT('Ctrl Pts',(9.58129688507772,0.698528137423855,9.58129688507772));
#31878=CARTESIAN_POINT('Ctrl Pts',(5.61259377015545,0.773528137423855,13.55));
#31879=CARTESIAN_POINT('Ctrl Pts',(0.,0.848528137423854,13.55));
#31880=CARTESIAN_POINT('Ctrl Pts',(-5.61259377015544,0.923528137423854,
13.55));
#31881=CARTESIAN_POINT('Ctrl Pts',(-9.58129688507772,0.998528137423854,
9.58129688507772));
#31882=CARTESIAN_POINT('Ctrl Pts',(-13.55,1.07352813742385,5.61259377015544));
#31883=CARTESIAN_POINT('Ctrl Pts',(-13.55,1.14852813742385,8.29698206422332E-16));
#31884=CARTESIAN_POINT('Ctrl Pts',(-13.55,1.22352813742385,-5.61259377015544));
#31885=CARTESIAN_POINT('Ctrl Pts',(-9.58129688507772,1.29852813742385,-9.58129688507772));
#31886=CARTESIAN_POINT('Ctrl Pts',(-5.61259377015544,1.37352813742385,-13.55));
#31887=CARTESIAN_POINT('Ctrl Pts',(-1.65939641284466E-15,1.44852813742385,
-13.55));
#31888=CARTESIAN_POINT('Ctrl Pts',(5.61259377015544,1.52352813742385,-13.55));
#31889=CARTESIAN_POINT('Ctrl Pts',(9.58129688507772,1.59852813742385,-9.58129688507772));
#31890=CARTESIAN_POINT('Ctrl Pts',(13.55,1.67352813742385,-5.61259377015545));
#31891=CARTESIAN_POINT('Ctrl Pts',(13.55,1.74852813742385,-2.489094619267E-15));
#31892=CARTESIAN_POINT('Ctrl Pts',(13.55,1.82352813742385,5.61259377015544));
#31893=CARTESIAN_POINT('Ctrl Pts',(9.58129688507772,1.89852813742385,9.58129688507772));
#31894=CARTESIAN_POINT('Ctrl Pts',(5.61259377015545,1.97352813742385,13.55));
#31895=CARTESIAN_POINT('Ctrl Pts',(0.,2.04852813742385,13.55));
#31896=CARTESIAN_POINT('Ctrl Pts',(-5.61259377015544,2.12352813742385,13.55));
#31897=CARTESIAN_POINT('Ctrl Pts',(-9.58129688507772,2.19852813742385,9.58129688507772));
#31898=CARTESIAN_POINT('Ctrl Pts',(-13.55,2.27352813742385,5.61259377015544));
#31899=CARTESIAN_POINT('Ctrl Pts',(-13.55,2.34852813742385,8.29698206422332E-16));
#31900=CARTESIAN_POINT('Ctrl Pts',(-13.55,2.42352813742385,-5.61259377015544));
#31901=CARTESIAN_POINT('Ctrl Pts',(-9.58129688507772,2.49852813742385,-9.58129688507772));
#31902=CARTESIAN_POINT('Ctrl Pts',(-5.61259377015544,2.57352813742385,-13.55));
#31903=CARTESIAN_POINT('Ctrl Pts',(-1.65939641284466E-15,2.64852813742385,
-13.55));
#31904=CARTESIAN_POINT('Ctrl Pts',(5.61259377015544,2.72352813742385,-13.55));
#31905=CARTESIAN_POINT('Ctrl Pts',(9.58129688507772,2.79852813742385,-9.58129688507772));
#31906=CARTESIAN_POINT('Ctrl Pts',(13.55,2.87352813742385,-5.61259377015545));
#31907=CARTESIAN_POINT('Ctrl Pts',(13.55,2.94852813742385,-2.489094619267E-15));
#31908=CARTESIAN_POINT('Ctrl Pts',(13.55,3.02352813742385,5.61259377015544));
#31909=CARTESIAN_POINT('Ctrl Pts',(9.58129688507772,3.09852813742385,9.58129688507772));
#31910=CARTESIAN_POINT('Ctrl Pts',(5.61259377015545,3.17352813742385,13.55));
#31911=CARTESIAN_POINT('Ctrl Pts',(0.,3.24852813742385,13.55));
#31912=CARTESIAN_POINT('Ctrl Pts',(-5.61259377015544,3.32352813742385,13.55));
#31913=CARTESIAN_POINT('Ctrl Pts',(-9.58129688507772,3.39852813742385,9.58129688507772));
#31914=CARTESIAN_POINT('Ctrl Pts',(-13.55,3.47352813742385,5.61259377015544));
#31915=CARTESIAN_POINT('Ctrl Pts',(-13.55,3.54852813742385,8.29698206422332E-16));
#31916=CARTESIAN_POINT('Ctrl Pts',(-13.55,3.62352813742385,-5.61259377015544));
#31917=CARTESIAN_POINT('Ctrl Pts',(-9.58129688507772,3.69852813742385,-9.58129688507772));
#31918=CARTESIAN_POINT('Ctrl Pts',(-5.61259377015544,3.77352813742385,-13.55));
#31919=CARTESIAN_POINT('Ctrl Pts',(-1.65939641284466E-15,3.84852813742385,
-13.55));
#31920=CARTESIAN_POINT('Ctrl Pts',(5.61259377015544,3.92352813742385,-13.55));
#31921=CARTESIAN_POINT('Ctrl Pts',(9.58129688507772,3.99852813742385,-9.58129688507772));
#31922=CARTESIAN_POINT('Ctrl Pts',(13.55,4.07352813742385,-5.61259377015545));
#31923=CARTESIAN_POINT('Ctrl Pts',(13.55,4.14852813742385,-2.489094619267E-15));
#31924=CARTESIAN_POINT('Ctrl Pts',(13.55,4.22352813742385,5.61259377015544));
#31925=CARTESIAN_POINT('Ctrl Pts',(9.58129688507772,4.29852813742385,9.58129688507772));
#31926=CARTESIAN_POINT('Ctrl Pts',(5.61259377015545,4.37352813742385,13.55));
#31927=CARTESIAN_POINT('Ctrl Pts',(0.,4.44852813742385,13.55));
#31928=CARTESIAN_POINT('Ctrl Pts',(0.,0.,13.55));
#31929=CARTESIAN_POINT('Ctrl Pts',(-5.61259377015544,0.0749999999999998,
13.55));
#31930=CARTESIAN_POINT('Ctrl Pts',(-9.58129688507772,0.15,9.58129688507772));
#31931=CARTESIAN_POINT('Ctrl Pts',(-13.55,0.225,5.61259377015544));
#31932=CARTESIAN_POINT('Ctrl Pts',(-13.55,0.299999999999999,8.29698206422332E-16));
#31933=CARTESIAN_POINT('Ctrl Pts',(-13.55,0.374999999999999,-5.61259377015544));
#31934=CARTESIAN_POINT('Ctrl Pts',(-9.58129688507772,0.449999999999999,
-9.58129688507772));
#31935=CARTESIAN_POINT('Ctrl Pts',(-5.61259377015544,0.524999999999999,
-13.55));
#31936=CARTESIAN_POINT('Ctrl Pts',(-1.65939641284466E-15,0.599999999999999,
-13.55));
#31937=CARTESIAN_POINT('Ctrl Pts',(5.61259377015543,0.674999999999998,-13.55));
#31938=CARTESIAN_POINT('Ctrl Pts',(9.58129688507772,0.749999999999998,-9.58129688507772));
#31939=CARTESIAN_POINT('Ctrl Pts',(13.55,0.824999999999998,-5.61259377015545));
#31940=CARTESIAN_POINT('Ctrl Pts',(13.55,0.899999999999998,-2.489094619267E-15));
#31941=CARTESIAN_POINT('Ctrl Pts',(13.55,0.974999999999998,5.61259377015544));
#31942=CARTESIAN_POINT('Ctrl Pts',(9.58129688507772,1.05,9.58129688507772));
#31943=CARTESIAN_POINT('Ctrl Pts',(5.61259377015545,1.125,13.55));
#31944=CARTESIAN_POINT('Ctrl Pts',(0.,1.2,13.55));
#31945=CARTESIAN_POINT('Ctrl Pts',(-5.61259377015544,1.275,13.55));
#31946=CARTESIAN_POINT('Ctrl Pts',(-9.58129688507772,1.35,9.58129688507772));
#31947=CARTESIAN_POINT('Ctrl Pts',(-13.55,1.425,5.61259377015544));
#31948=CARTESIAN_POINT('Ctrl Pts',(-13.55,1.5,8.29698206422332E-16));
#31949=CARTESIAN_POINT('Ctrl Pts',(-13.55,1.575,-5.61259377015544));
#31950=CARTESIAN_POINT('Ctrl Pts',(-9.58129688507772,1.65,-9.58129688507772));
#31951=CARTESIAN_POINT('Ctrl Pts',(-5.61259377015544,1.725,-13.55));
#31952=CARTESIAN_POINT('Ctrl Pts',(-1.65939641284466E-15,1.8,-13.55));
#31953=CARTESIAN_POINT('Ctrl Pts',(5.61259377015543,1.875,-13.55));
#31954=CARTESIAN_POINT('Ctrl Pts',(9.58129688507772,1.95,-9.58129688507772));
#31955=CARTESIAN_POINT('Ctrl Pts',(13.55,2.025,-5.61259377015545));
#31956=CARTESIAN_POINT('Ctrl Pts',(13.55,2.1,-2.489094619267E-15));
#31957=CARTESIAN_POINT('Ctrl Pts',(13.55,2.17499999999999,5.61259377015544));
#31958=CARTESIAN_POINT('Ctrl Pts',(9.58129688507772,2.25,9.58129688507772));
#31959=CARTESIAN_POINT('Ctrl Pts',(5.61259377015545,2.32499999999999,13.55));
#31960=CARTESIAN_POINT('Ctrl Pts',(0.,2.39999999999999,13.55));
#31961=CARTESIAN_POINT('Ctrl Pts',(-5.61259377015544,2.47499999999999,13.55));
#31962=CARTESIAN_POINT('Ctrl Pts',(-9.58129688507772,2.54999999999999,9.58129688507772));
#31963=CARTESIAN_POINT('Ctrl Pts',(-13.55,2.62499999999999,5.61259377015544));
#31964=CARTESIAN_POINT('Ctrl Pts',(-13.55,2.69999999999999,8.29698206422332E-16));
#31965=CARTESIAN_POINT('Ctrl Pts',(-13.55,2.77499999999999,-5.61259377015544));
#31966=CARTESIAN_POINT('Ctrl Pts',(-9.58129688507772,2.84999999999999,-9.58129688507772));
#31967=CARTESIAN_POINT('Ctrl Pts',(-5.61259377015544,2.92499999999999,-13.55));
#31968=CARTESIAN_POINT('Ctrl Pts',(-1.65939641284466E-15,2.99999999999999,
-13.55));
#31969=CARTESIAN_POINT('Ctrl Pts',(5.61259377015543,3.07499999999999,-13.55));
#31970=CARTESIAN_POINT('Ctrl Pts',(9.58129688507772,3.14999999999999,-9.58129688507772));
#31971=CARTESIAN_POINT('Ctrl Pts',(13.55,3.22499999999999,-5.61259377015545));
#31972=CARTESIAN_POINT('Ctrl Pts',(13.55,3.29999999999999,-2.489094619267E-15));
#31973=CARTESIAN_POINT('Ctrl Pts',(13.55,3.37499999999999,5.61259377015544));
#31974=CARTESIAN_POINT('Ctrl Pts',(9.58129688507772,3.44999999999999,9.58129688507772));
#31975=CARTESIAN_POINT('Ctrl Pts',(5.61259377015545,3.52499999999999,13.55));
#31976=CARTESIAN_POINT('Ctrl Pts',(0.,3.59999999999999,13.55));
#31977=CARTESIAN_POINT('Ctrl Pts',(-5.61259377015544,3.67499999999999,13.55));
#31978=CARTESIAN_POINT('Ctrl Pts',(-9.58129688507772,3.74999999999999,9.58129688507772));
#31979=CARTESIAN_POINT('Ctrl Pts',(-13.55,3.82499999999999,5.61259377015544));
#31980=CARTESIAN_POINT('Ctrl Pts',(-13.55,3.89999999999999,8.29698206422332E-16));
#31981=CARTESIAN_POINT('Ctrl Pts',(-13.55,3.97499999999999,-5.61259377015544));
#31982=CARTESIAN_POINT('Ctrl Pts',(-9.58129688507772,4.04999999999999,-9.58129688507772));
#31983=CARTESIAN_POINT('Ctrl Pts',(-5.61259377015544,4.12499999999999,-13.55));
#31984=CARTESIAN_POINT('Ctrl Pts',(-1.65939641284466E-15,4.19999999999999,
-13.55));
#31985=CARTESIAN_POINT('Ctrl Pts',(5.61259377015543,4.27499999999999,-13.55));
#31986=CARTESIAN_POINT('Ctrl Pts',(9.58129688507772,4.34999999999999,-9.58129688507772));
#31987=CARTESIAN_POINT('Ctrl Pts',(13.55,4.42499999999999,-5.61259377015545));
#31988=CARTESIAN_POINT('Ctrl Pts',(13.55,4.49999999999999,-2.489094619267E-15));
#31989=CARTESIAN_POINT('Ctrl Pts',(13.55,4.57499999999999,5.61259377015544));
#31990=CARTESIAN_POINT('Ctrl Pts',(9.58129688507772,4.64999999999999,9.58129688507772));
#31991=CARTESIAN_POINT('Ctrl Pts',(5.61259377015545,4.72499999999999,13.55));
#31992=CARTESIAN_POINT('Ctrl Pts',(0.,4.79999999999999,13.55));
#31993=CARTESIAN_POINT('',(-1.7328752207935E-15,-0.599999999999999,14.15));
#31994=CARTESIAN_POINT('Origin',(0.,0.,14.15));
#31995=CARTESIAN_POINT('Ctrl Pts',(-1.7328752207935E-15,-0.599999999999999,
14.15));
#31996=CARTESIAN_POINT('Ctrl Pts',(-5.8611219075793,-0.524999999999999,
14.15));
#31997=CARTESIAN_POINT('Ctrl Pts',(-10.0055609537896,-0.449999999999999,
10.0055609537896));
#31998=CARTESIAN_POINT('Ctrl Pts',(-14.15,-0.374999999999999,5.86112190757929));
#31999=CARTESIAN_POINT('Ctrl Pts',(-14.15,-0.299999999999999,-8.66437610396752E-16));
#32000=CARTESIAN_POINT('Ctrl Pts',(-14.15,-0.225,-5.8611219075793));
#32001=CARTESIAN_POINT('Ctrl Pts',(-10.0055609537896,-0.15,-10.0055609537896));
#32002=CARTESIAN_POINT('Ctrl Pts',(-5.8611219075793,-0.0749999999999999,
-14.15));
#32003=CARTESIAN_POINT('Ctrl Pts',(0.,0.,-14.15));
#32004=CARTESIAN_POINT('Ctrl Pts',(5.86112190757929,0.0749999999999999,
-14.15));
#32005=CARTESIAN_POINT('Ctrl Pts',(10.0055609537896,0.15,-10.0055609537896));
#32006=CARTESIAN_POINT('Ctrl Pts',(14.15,0.225,-5.8611219075793));
#32007=CARTESIAN_POINT('Ctrl Pts',(14.15,0.299999999999999,-8.66437610396752E-16));
#32008=CARTESIAN_POINT('Ctrl Pts',(14.15,0.374999999999999,5.8611219075793));
#32009=CARTESIAN_POINT('Ctrl Pts',(10.0055609537896,0.449999999999999,10.0055609537896));
#32010=CARTESIAN_POINT('Ctrl Pts',(5.8611219075793,0.524999999999999,14.15));
#32011=CARTESIAN_POINT('Ctrl Pts',(1.7328752207935E-15,0.599999999999999,
14.15));
#32012=CARTESIAN_POINT('Ctrl Pts',(1.7328752207935E-15,0.599999999999999,
14.15));
#32013=CARTESIAN_POINT('Ctrl Pts',(-5.86112190757929,0.674999999999999,
14.15));
#32014=CARTESIAN_POINT('Ctrl Pts',(-10.0055609537896,0.749999999999998,
10.0055609537896));
#32015=CARTESIAN_POINT('Ctrl Pts',(-14.15,0.824999999999999,5.8611219075793));
#32016=CARTESIAN_POINT('Ctrl Pts',(-14.15,0.899999999999998,2.59931283119026E-15));
#32017=CARTESIAN_POINT('Ctrl Pts',(-14.15,0.974999999999998,-5.86112190757929));
#32018=CARTESIAN_POINT('Ctrl Pts',(-10.0055609537896,1.05,-10.0055609537896));
#32019=CARTESIAN_POINT('Ctrl Pts',(-5.8611219075793,1.125,-14.15));
#32020=CARTESIAN_POINT('Ctrl Pts',(-3.46575044158701E-15,1.2,-14.15));
#32021=CARTESIAN_POINT('Ctrl Pts',(5.86112190757929,1.275,-14.15));
#32022=CARTESIAN_POINT('Ctrl Pts',(10.0055609537896,1.35,-10.0055609537897));
#32023=CARTESIAN_POINT('Ctrl Pts',(14.15,1.425,-5.8611219075793));
#32024=CARTESIAN_POINT('Ctrl Pts',(14.15,1.5,-4.33218805198376E-15));
#32025=CARTESIAN_POINT('Ctrl Pts',(14.15,1.575,5.8611219075793));
#32026=CARTESIAN_POINT('Ctrl Pts',(10.0055609537897,1.65,10.0055609537896));
#32027=CARTESIAN_POINT('Ctrl Pts',(5.86112190757931,1.725,14.15));
#32028=CARTESIAN_POINT('Ctrl Pts',(5.19862566238051E-15,1.8,14.15));
#32029=CARTESIAN_POINT('Ctrl Pts',(-5.8611219075793,1.875,14.15));
#32030=CARTESIAN_POINT('Ctrl Pts',(-10.0055609537896,1.95,10.0055609537897));
#32031=CARTESIAN_POINT('Ctrl Pts',(-14.15,2.025,5.86112190757931));
#32032=CARTESIAN_POINT('Ctrl Pts',(-14.15,2.1,6.06506327277727E-15));
#32033=CARTESIAN_POINT('Ctrl Pts',(-14.15,2.175,-5.8611219075793));
#32034=CARTESIAN_POINT('Ctrl Pts',(-10.0055609537897,2.25,-10.0055609537896));
#32035=CARTESIAN_POINT('Ctrl Pts',(-5.86112190757931,2.32499999999999,-14.15));
#32036=CARTESIAN_POINT('Ctrl Pts',(-6.93150088317402E-15,2.4,-14.15));
#32037=CARTESIAN_POINT('Ctrl Pts',(5.86112190757929,2.475,-14.15));
#32038=CARTESIAN_POINT('Ctrl Pts',(10.0055609537896,2.54999999999999,-10.0055609537896));
#32039=CARTESIAN_POINT('Ctrl Pts',(14.15,2.625,-5.86112190757931));
#32040=CARTESIAN_POINT('Ctrl Pts',(14.15,2.69999999999999,-7.79793849357077E-15));
#32041=CARTESIAN_POINT('Ctrl Pts',(14.15,2.77499999999999,5.86112190757929));
#32042=CARTESIAN_POINT('Ctrl Pts',(10.0055609537897,2.84999999999999,10.0055609537896));
#32043=CARTESIAN_POINT('Ctrl Pts',(5.86112190757931,2.92499999999999,14.15));
#32044=CARTESIAN_POINT('Ctrl Pts',(8.66437610396752E-15,2.99999999999999,
14.15));
#32045=CARTESIAN_POINT('Ctrl Pts',(-5.86112190757929,3.07499999999999,14.15));
#32046=CARTESIAN_POINT('Ctrl Pts',(-10.0055609537896,3.14999999999999,10.0055609537896));
#32047=CARTESIAN_POINT('Ctrl Pts',(-14.15,3.22499999999999,5.86112190757931));
#32048=CARTESIAN_POINT('Ctrl Pts',(-14.15,3.29999999999999,9.53081371436428E-15));
#32049=CARTESIAN_POINT('Ctrl Pts',(-14.15,3.37499999999999,-5.86112190757929));
#32050=CARTESIAN_POINT('Ctrl Pts',(-10.0055609537897,3.44999999999999,-10.0055609537896));
#32051=CARTESIAN_POINT('Ctrl Pts',(-5.86112190757931,3.52499999999999,-14.15));
#32052=CARTESIAN_POINT('Ctrl Pts',(-1.0397251324761E-14,3.59999999999999,
-14.15));
#32053=CARTESIAN_POINT('Ctrl Pts',(5.86112190757927,3.67499999999999,-14.15));
#32054=CARTESIAN_POINT('Ctrl Pts',(10.0055609537896,3.74999999999999,-10.0055609537896));
#32055=CARTESIAN_POINT('Ctrl Pts',(14.15,3.82499999999999,-5.86112190757931));
#32056=CARTESIAN_POINT('Ctrl Pts',(14.15,3.89999999999999,-3.63991382126713E-14));
#32057=CARTESIAN_POINT('Ctrl Pts',(14.15,3.97499999999999,5.86112190757929));
#32058=CARTESIAN_POINT('Ctrl Pts',(10.0055609537897,4.04999999999999,10.0055609537896));
#32059=CARTESIAN_POINT('Ctrl Pts',(5.86112190757929,4.12499999999999,14.15));
#32060=CARTESIAN_POINT('Ctrl Pts',(1.21301265455545E-14,4.19999999999999,
14.15));
#32061=CARTESIAN_POINT('Origin',(-7.90471375114085E-13,4.8,14.15));
#32062=CARTESIAN_POINT('Ctrl Pts',(0.,7.34788079488412E-17,14.75));
#32063=CARTESIAN_POINT('Ctrl Pts',(-6.10965004500315,0.0749999999999999,
14.75));
#32064=CARTESIAN_POINT('Ctrl Pts',(-10.4298250225016,0.15,10.4298250225016));
#32065=CARTESIAN_POINT('Ctrl Pts',(-14.75,0.225,6.10965004500315));
#32066=CARTESIAN_POINT('Ctrl Pts',(-14.75,0.299999999999999,9.03177014371173E-16));
#32067=CARTESIAN_POINT('Ctrl Pts',(-14.75,0.374999999999999,-6.10965004500315));
#32068=CARTESIAN_POINT('Ctrl Pts',(-10.4298250225016,0.449999999999999,
-10.4298250225016));
#32069=CARTESIAN_POINT('Ctrl Pts',(-6.10965004500315,0.524999999999999,
-14.75));
#32070=CARTESIAN_POINT('Ctrl Pts',(-1.80635402874235E-15,0.599999999999999,
-14.75));
#32071=CARTESIAN_POINT('Ctrl Pts',(6.10965004500315,0.674999999999999,-14.75));
#32072=CARTESIAN_POINT('Ctrl Pts',(10.4298250225016,0.749999999999998,-10.4298250225016));
#32073=CARTESIAN_POINT('Ctrl Pts',(14.75,0.824999999999999,-6.10965004500316));
#32074=CARTESIAN_POINT('Ctrl Pts',(14.75,0.899999999999998,-2.70953104311352E-15));
#32075=CARTESIAN_POINT('Ctrl Pts',(14.75,0.974999999999998,6.10965004500316));
#32076=CARTESIAN_POINT('Ctrl Pts',(10.4298250225016,1.05,10.4298250225016));
#32077=CARTESIAN_POINT('Ctrl Pts',(6.10965004500316,1.125,14.75));
#32078=CARTESIAN_POINT('Ctrl Pts',(0.,1.2,14.75));
#32079=CARTESIAN_POINT('Ctrl Pts',(-6.10965004500315,1.275,14.75));
#32080=CARTESIAN_POINT('Ctrl Pts',(-10.4298250225016,1.35,10.4298250225016));
#32081=CARTESIAN_POINT('Ctrl Pts',(-14.75,1.425,6.10965004500315));
#32082=CARTESIAN_POINT('Ctrl Pts',(-14.75,1.5,9.03177014371173E-16));
#32083=CARTESIAN_POINT('Ctrl Pts',(-14.75,1.575,-6.10965004500315));
#32084=CARTESIAN_POINT('Ctrl Pts',(-10.4298250225016,1.65,-10.4298250225016));
#32085=CARTESIAN_POINT('Ctrl Pts',(-6.10965004500315,1.725,-14.75));
#32086=CARTESIAN_POINT('Ctrl Pts',(-1.80635402874235E-15,1.8,-14.75));
#32087=CARTESIAN_POINT('Ctrl Pts',(6.10965004500315,1.875,-14.75));
#32088=CARTESIAN_POINT('Ctrl Pts',(10.4298250225016,1.95,-10.4298250225016));
#32089=CARTESIAN_POINT('Ctrl Pts',(14.75,2.025,-6.10965004500316));
#32090=CARTESIAN_POINT('Ctrl Pts',(14.75,2.1,-2.70953104311352E-15));
#32091=CARTESIAN_POINT('Ctrl Pts',(14.75,2.17499999999999,6.10965004500316));
#32092=CARTESIAN_POINT('Ctrl Pts',(10.4298250225016,2.25,10.4298250225016));
#32093=CARTESIAN_POINT('Ctrl Pts',(6.10965004500316,2.32499999999999,14.75));
#32094=CARTESIAN_POINT('Ctrl Pts',(0.,2.39999999999999,14.75));
#32095=CARTESIAN_POINT('Ctrl Pts',(-6.10965004500315,2.47499999999999,14.75));
#32096=CARTESIAN_POINT('Ctrl Pts',(-10.4298250225016,2.54999999999999,10.4298250225016));
#32097=CARTESIAN_POINT('Ctrl Pts',(-14.75,2.62499999999999,6.10965004500315));
#32098=CARTESIAN_POINT('Ctrl Pts',(-14.75,2.69999999999999,9.03177014371173E-16));
#32099=CARTESIAN_POINT('Ctrl Pts',(-14.75,2.77499999999999,-6.10965004500315));
#32100=CARTESIAN_POINT('Ctrl Pts',(-10.4298250225016,2.84999999999999,-10.4298250225016));
#32101=CARTESIAN_POINT('Ctrl Pts',(-6.10965004500315,2.92499999999999,-14.75));
#32102=CARTESIAN_POINT('Ctrl Pts',(-1.80635402874235E-15,2.99999999999999,
-14.75));
#32103=CARTESIAN_POINT('Ctrl Pts',(6.10965004500315,3.07499999999999,-14.75));
#32104=CARTESIAN_POINT('Ctrl Pts',(10.4298250225016,3.14999999999999,-10.4298250225016));
#32105=CARTESIAN_POINT('Ctrl Pts',(14.75,3.22499999999999,-6.10965004500316));
#32106=CARTESIAN_POINT('Ctrl Pts',(14.75,3.29999999999999,-2.70953104311352E-15));
#32107=CARTESIAN_POINT('Ctrl Pts',(14.75,3.37499999999999,6.10965004500316));
#32108=CARTESIAN_POINT('Ctrl Pts',(10.4298250225016,3.44999999999999,10.4298250225016));
#32109=CARTESIAN_POINT('Ctrl Pts',(6.10965004500316,3.52499999999999,14.75));
#32110=CARTESIAN_POINT('Ctrl Pts',(0.,3.59999999999999,14.75));
#32111=CARTESIAN_POINT('Ctrl Pts',(-6.10965004500315,3.67499999999999,14.75));
#32112=CARTESIAN_POINT('Ctrl Pts',(-10.4298250225016,3.74999999999999,10.4298250225016));
#32113=CARTESIAN_POINT('Ctrl Pts',(-14.75,3.82499999999999,6.10965004500315));
#32114=CARTESIAN_POINT('Ctrl Pts',(-14.75,3.89999999999999,9.03177014371173E-16));
#32115=CARTESIAN_POINT('Ctrl Pts',(-14.75,3.97499999999999,-6.10965004500315));
#32116=CARTESIAN_POINT('Ctrl Pts',(-10.4298250225016,4.04999999999999,-10.4298250225016));
#32117=CARTESIAN_POINT('Ctrl Pts',(-6.10965004500315,4.12499999999999,-14.75));
#32118=CARTESIAN_POINT('Ctrl Pts',(-1.80635402874235E-15,4.19999999999999,
-14.75));
#32119=CARTESIAN_POINT('Ctrl Pts',(6.10965004500315,4.27499999999999,-14.75));
#32120=CARTESIAN_POINT('Ctrl Pts',(10.4298250225016,4.34999999999999,-10.4298250225016));
#32121=CARTESIAN_POINT('Ctrl Pts',(14.75,4.42499999999999,-6.10965004500316));
#32122=CARTESIAN_POINT('Ctrl Pts',(14.75,4.49999999999999,-2.70953104311352E-15));
#32123=CARTESIAN_POINT('Ctrl Pts',(14.75,4.57499999999999,6.10965004500316));
#32124=CARTESIAN_POINT('Ctrl Pts',(10.4298250225016,4.64999999999999,10.4298250225016));
#32125=CARTESIAN_POINT('Ctrl Pts',(6.10965004500316,4.72499999999999,14.75));
#32126=CARTESIAN_POINT('Ctrl Pts',(0.,4.79999999999999,14.75));
#32127=CARTESIAN_POINT('Ctrl Pts',(0.,-0.351471862576143,14.75));
#32128=CARTESIAN_POINT('Ctrl Pts',(-6.10965004500315,-0.276471862576143,
14.75));
#32129=CARTESIAN_POINT('Ctrl Pts',(-10.4298250225016,-0.201471862576143,
10.4298250225016));
#32130=CARTESIAN_POINT('Ctrl Pts',(-14.75,-0.126471862576144,6.10965004500315));
#32131=CARTESIAN_POINT('Ctrl Pts',(-14.75,-0.0514718625761437,9.03177014371173E-16));
#32132=CARTESIAN_POINT('Ctrl Pts',(-14.75,0.0235281374238561,-6.10965004500315));
#32133=CARTESIAN_POINT('Ctrl Pts',(-10.4298250225016,0.098528137423856,
-10.4298250225016));
#32134=CARTESIAN_POINT('Ctrl Pts',(-6.10965004500315,0.173528137423856,
-14.75));
#32135=CARTESIAN_POINT('Ctrl Pts',(-1.80635402874235E-15,0.248528137423856,
-14.75));
#32136=CARTESIAN_POINT('Ctrl Pts',(6.10965004500315,0.323528137423855,-14.75));
#32137=CARTESIAN_POINT('Ctrl Pts',(10.4298250225016,0.398528137423855,-10.4298250225016));
#32138=CARTESIAN_POINT('Ctrl Pts',(14.75,0.473528137423855,-6.10965004500316));
#32139=CARTESIAN_POINT('Ctrl Pts',(14.75,0.548528137423855,-2.70953104311352E-15));
#32140=CARTESIAN_POINT('Ctrl Pts',(14.75,0.623528137423855,6.10965004500316));
#32141=CARTESIAN_POINT('Ctrl Pts',(10.4298250225016,0.698528137423855,10.4298250225016));
#32142=CARTESIAN_POINT('Ctrl Pts',(6.10965004500316,0.773528137423855,14.75));
#32143=CARTESIAN_POINT('Ctrl Pts',(0.,0.848528137423854,14.75));
#32144=CARTESIAN_POINT('Ctrl Pts',(-6.10965004500315,0.923528137423854,
14.75));
#32145=CARTESIAN_POINT('Ctrl Pts',(-10.4298250225016,0.998528137423854,
10.4298250225016));
#32146=CARTESIAN_POINT('Ctrl Pts',(-14.75,1.07352813742385,6.10965004500315));
#32147=CARTESIAN_POINT('Ctrl Pts',(-14.75,1.14852813742385,9.03177014371173E-16));
#32148=CARTESIAN_POINT('Ctrl Pts',(-14.75,1.22352813742385,-6.10965004500315));
#32149=CARTESIAN_POINT('Ctrl Pts',(-10.4298250225016,1.29852813742385,-10.4298250225016));
#32150=CARTESIAN_POINT('Ctrl Pts',(-6.10965004500315,1.37352813742385,-14.75));
#32151=CARTESIAN_POINT('Ctrl Pts',(-1.80635402874235E-15,1.44852813742385,
-14.75));
#32152=CARTESIAN_POINT('Ctrl Pts',(6.10965004500315,1.52352813742385,-14.75));
#32153=CARTESIAN_POINT('Ctrl Pts',(10.4298250225016,1.59852813742385,-10.4298250225016));
#32154=CARTESIAN_POINT('Ctrl Pts',(14.75,1.67352813742385,-6.10965004500316));
#32155=CARTESIAN_POINT('Ctrl Pts',(14.75,1.74852813742385,-2.70953104311352E-15));
#32156=CARTESIAN_POINT('Ctrl Pts',(14.75,1.82352813742385,6.10965004500316));
#32157=CARTESIAN_POINT('Ctrl Pts',(10.4298250225016,1.89852813742385,10.4298250225016));
#32158=CARTESIAN_POINT('Ctrl Pts',(6.10965004500316,1.97352813742385,14.75));
#32159=CARTESIAN_POINT('Ctrl Pts',(0.,2.04852813742385,14.75));
#32160=CARTESIAN_POINT('Ctrl Pts',(-6.10965004500315,2.12352813742385,14.75));
#32161=CARTESIAN_POINT('Ctrl Pts',(-10.4298250225016,2.19852813742385,10.4298250225016));
#32162=CARTESIAN_POINT('Ctrl Pts',(-14.75,2.27352813742385,6.10965004500315));
#32163=CARTESIAN_POINT('Ctrl Pts',(-14.75,2.34852813742385,9.03177014371173E-16));
#32164=CARTESIAN_POINT('Ctrl Pts',(-14.75,2.42352813742385,-6.10965004500315));
#32165=CARTESIAN_POINT('Ctrl Pts',(-10.4298250225016,2.49852813742385,-10.4298250225016));
#32166=CARTESIAN_POINT('Ctrl Pts',(-6.10965004500315,2.57352813742385,-14.75));
#32167=CARTESIAN_POINT('Ctrl Pts',(-1.80635402874235E-15,2.64852813742385,
-14.75));
#32168=CARTESIAN_POINT('Ctrl Pts',(6.10965004500315,2.72352813742385,-14.75));
#32169=CARTESIAN_POINT('Ctrl Pts',(10.4298250225016,2.79852813742385,-10.4298250225016));
#32170=CARTESIAN_POINT('Ctrl Pts',(14.75,2.87352813742385,-6.10965004500316));
#32171=CARTESIAN_POINT('Ctrl Pts',(14.75,2.94852813742385,-2.70953104311352E-15));
#32172=CARTESIAN_POINT('Ctrl Pts',(14.75,3.02352813742385,6.10965004500316));
#32173=CARTESIAN_POINT('Ctrl Pts',(10.4298250225016,3.09852813742385,10.4298250225016));
#32174=CARTESIAN_POINT('Ctrl Pts',(6.10965004500316,3.17352813742385,14.75));
#32175=CARTESIAN_POINT('Ctrl Pts',(0.,3.24852813742385,14.75));
#32176=CARTESIAN_POINT('Ctrl Pts',(-6.10965004500315,3.32352813742385,14.75));
#32177=CARTESIAN_POINT('Ctrl Pts',(-10.4298250225016,3.39852813742385,10.4298250225016));
#32178=CARTESIAN_POINT('Ctrl Pts',(-14.75,3.47352813742385,6.10965004500315));
#32179=CARTESIAN_POINT('Ctrl Pts',(-14.75,3.54852813742385,9.03177014371173E-16));
#32180=CARTESIAN_POINT('Ctrl Pts',(-14.75,3.62352813742385,-6.10965004500315));
#32181=CARTESIAN_POINT('Ctrl Pts',(-10.4298250225016,3.69852813742385,-10.4298250225016));
#32182=CARTESIAN_POINT('Ctrl Pts',(-6.10965004500315,3.77352813742385,-14.75));
#32183=CARTESIAN_POINT('Ctrl Pts',(-1.80635402874235E-15,3.84852813742385,
-14.75));
#32184=CARTESIAN_POINT('Ctrl Pts',(6.10965004500315,3.92352813742385,-14.75));
#32185=CARTESIAN_POINT('Ctrl Pts',(10.4298250225016,3.99852813742385,-10.4298250225016));
#32186=CARTESIAN_POINT('Ctrl Pts',(14.75,4.07352813742385,-6.10965004500316));
#32187=CARTESIAN_POINT('Ctrl Pts',(14.75,4.14852813742385,-2.70953104311352E-15));
#32188=CARTESIAN_POINT('Ctrl Pts',(14.75,4.22352813742385,6.10965004500316));
#32189=CARTESIAN_POINT('Ctrl Pts',(10.4298250225016,4.29852813742385,10.4298250225016));
#32190=CARTESIAN_POINT('Ctrl Pts',(6.10965004500316,4.37352813742385,14.75));
#32191=CARTESIAN_POINT('Ctrl Pts',(0.,4.44852813742385,14.75));
#32192=CARTESIAN_POINT('Ctrl Pts',(0.,-0.6,14.5014718625761));
#32193=CARTESIAN_POINT('Ctrl Pts',(-6.00670631985087,-0.525,14.5014718625761));
#32194=CARTESIAN_POINT('Ctrl Pts',(-10.2540890912135,-0.45,10.2540890912135));
#32195=CARTESIAN_POINT('Ctrl Pts',(-14.5014718625761,-0.375000000000001,
6.00670631985087));
#32196=CARTESIAN_POINT('Ctrl Pts',(-14.5014718625761,-0.300000000000001,
8.87959054971464E-16));
#32197=CARTESIAN_POINT('Ctrl Pts',(-14.5014718625761,-0.225000000000001,
-6.00670631985087));
#32198=CARTESIAN_POINT('Ctrl Pts',(-10.2540890912135,-0.150000000000001,
-10.2540890912135));
#32199=CARTESIAN_POINT('Ctrl Pts',(-6.00670631985087,-0.0750000000000013,
-14.5014718625761));
#32200=CARTESIAN_POINT('Ctrl Pts',(-1.77591810994293E-15,-1.40946282423116E-15,
-14.5014718625761));
#32201=CARTESIAN_POINT('Ctrl Pts',(6.00670631985087,0.0749999999999985,
-14.5014718625761));
#32202=CARTESIAN_POINT('Ctrl Pts',(10.2540890912135,0.149999999999998,-10.2540890912135));
#32203=CARTESIAN_POINT('Ctrl Pts',(14.5014718625761,0.224999999999998,-6.00670631985087));
#32204=CARTESIAN_POINT('Ctrl Pts',(14.5014718625761,0.299999999999998,-2.66387716491439E-15));
#32205=CARTESIAN_POINT('Ctrl Pts',(14.5014718625761,0.374999999999998,6.00670631985087));
#32206=CARTESIAN_POINT('Ctrl Pts',(10.2540890912135,0.449999999999998,10.2540890912135));
#32207=CARTESIAN_POINT('Ctrl Pts',(6.00670631985088,0.524999999999997,14.5014718625761));
#32208=CARTESIAN_POINT('Ctrl Pts',(0.,0.599999999999997,14.5014718625761));
#32209=CARTESIAN_POINT('Ctrl Pts',(-6.00670631985087,0.674999999999997,
14.5014718625761));
#32210=CARTESIAN_POINT('Ctrl Pts',(-10.2540890912135,0.749999999999997,
10.2540890912135));
#32211=CARTESIAN_POINT('Ctrl Pts',(-14.5014718625761,0.824999999999997,
6.00670631985087));
#32212=CARTESIAN_POINT('Ctrl Pts',(-14.5014718625761,0.899999999999996,
8.87959054971464E-16));
#32213=CARTESIAN_POINT('Ctrl Pts',(-14.5014718625761,0.974999999999997,
-6.00670631985087));
#32214=CARTESIAN_POINT('Ctrl Pts',(-10.2540890912135,1.05,-10.2540890912135));
#32215=CARTESIAN_POINT('Ctrl Pts',(-6.00670631985087,1.125,-14.5014718625761));
#32216=CARTESIAN_POINT('Ctrl Pts',(-1.77591810994293E-15,1.2,-14.5014718625761));
#32217=CARTESIAN_POINT('Ctrl Pts',(6.00670631985087,1.275,-14.5014718625761));
#32218=CARTESIAN_POINT('Ctrl Pts',(10.2540890912135,1.35,-10.2540890912135));
#32219=CARTESIAN_POINT('Ctrl Pts',(14.5014718625761,1.425,-6.00670631985087));
#32220=CARTESIAN_POINT('Ctrl Pts',(14.5014718625761,1.5,-2.66387716491439E-15));
#32221=CARTESIAN_POINT('Ctrl Pts',(14.5014718625761,1.575,6.00670631985087));
#32222=CARTESIAN_POINT('Ctrl Pts',(10.2540890912135,1.65,10.2540890912135));
#32223=CARTESIAN_POINT('Ctrl Pts',(6.00670631985088,1.72499999999999,14.5014718625761));
#32224=CARTESIAN_POINT('Ctrl Pts',(0.,1.79999999999999,14.5014718625761));
#32225=CARTESIAN_POINT('Ctrl Pts',(-6.00670631985087,1.87499999999999,14.5014718625761));
#32226=CARTESIAN_POINT('Ctrl Pts',(-10.2540890912135,1.94999999999999,10.2540890912135));
#32227=CARTESIAN_POINT('Ctrl Pts',(-14.5014718625761,2.02499999999999,6.00670631985087));
#32228=CARTESIAN_POINT('Ctrl Pts',(-14.5014718625761,2.09999999999999,8.87959054971464E-16));
#32229=CARTESIAN_POINT('Ctrl Pts',(-14.5014718625761,2.17499999999999,-6.00670631985087));
#32230=CARTESIAN_POINT('Ctrl Pts',(-10.2540890912135,2.24999999999999,-10.2540890912135));
#32231=CARTESIAN_POINT('Ctrl Pts',(-6.00670631985087,2.32499999999999,-14.5014718625761));
#32232=CARTESIAN_POINT('Ctrl Pts',(-1.77591810994293E-15,2.39999999999999,
-14.5014718625761));
#32233=CARTESIAN_POINT('Ctrl Pts',(6.00670631985087,2.47499999999999,-14.5014718625761));
#32234=CARTESIAN_POINT('Ctrl Pts',(10.2540890912135,2.54999999999999,-10.2540890912135));
#32235=CARTESIAN_POINT('Ctrl Pts',(14.5014718625761,2.62499999999999,-6.00670631985087));
#32236=CARTESIAN_POINT('Ctrl Pts',(14.5014718625761,2.69999999999999,-2.66387716491439E-15));
#32237=CARTESIAN_POINT('Ctrl Pts',(14.5014718625761,2.77499999999999,6.00670631985087));
#32238=CARTESIAN_POINT('Ctrl Pts',(10.2540890912135,2.84999999999999,10.2540890912135));
#32239=CARTESIAN_POINT('Ctrl Pts',(6.00670631985088,2.92499999999999,14.5014718625761));
#32240=CARTESIAN_POINT('Ctrl Pts',(0.,2.99999999999999,14.5014718625761));
#32241=CARTESIAN_POINT('Ctrl Pts',(-6.00670631985087,3.07499999999999,14.5014718625761));
#32242=CARTESIAN_POINT('Ctrl Pts',(-10.2540890912135,3.14999999999999,10.2540890912135));
#32243=CARTESIAN_POINT('Ctrl Pts',(-14.5014718625761,3.22499999999999,6.00670631985087));
#32244=CARTESIAN_POINT('Ctrl Pts',(-14.5014718625761,3.29999999999999,8.87959054971464E-16));
#32245=CARTESIAN_POINT('Ctrl Pts',(-14.5014718625761,3.37499999999999,-6.00670631985087));
#32246=CARTESIAN_POINT('Ctrl Pts',(-10.2540890912135,3.44999999999999,-10.2540890912135));
#32247=CARTESIAN_POINT('Ctrl Pts',(-6.00670631985087,3.52499999999999,-14.5014718625761));
#32248=CARTESIAN_POINT('Ctrl Pts',(-1.77591810994293E-15,3.59999999999999,
-14.5014718625761));
#32249=CARTESIAN_POINT('Ctrl Pts',(6.00670631985087,3.67499999999999,-14.5014718625761));
#32250=CARTESIAN_POINT('Ctrl Pts',(10.2540890912135,3.74999999999999,-10.2540890912135));
#32251=CARTESIAN_POINT('Ctrl Pts',(14.5014718625761,3.82499999999999,-6.00670631985087));
#32252=CARTESIAN_POINT('Ctrl Pts',(14.5014718625761,3.89999999999999,-2.66387716491439E-15));
#32253=CARTESIAN_POINT('Ctrl Pts',(14.5014718625761,3.97499999999999,6.00670631985087));
#32254=CARTESIAN_POINT('Ctrl Pts',(10.2540890912135,4.04999999999999,10.2540890912135));
#32255=CARTESIAN_POINT('Ctrl Pts',(6.00670631985088,4.12499999999999,14.5014718625761));
#32256=CARTESIAN_POINT('Ctrl Pts',(0.,4.19999999999999,14.5014718625761));
#32257=CARTESIAN_POINT('Ctrl Pts',(0.,-0.6,14.15));
#32258=CARTESIAN_POINT('Ctrl Pts',(-5.8611219075793,-0.525,14.15));
#32259=CARTESIAN_POINT('Ctrl Pts',(-10.0055609537896,-0.450000000000001,
10.0055609537896));
#32260=CARTESIAN_POINT('Ctrl Pts',(-14.15,-0.375000000000001,5.8611219075793));
#32261=CARTESIAN_POINT('Ctrl Pts',(-14.15,-0.300000000000001,8.66437610396752E-16));
#32262=CARTESIAN_POINT('Ctrl Pts',(-14.15,-0.225000000000001,-5.86112190757929));
#32263=CARTESIAN_POINT('Ctrl Pts',(-10.0055609537896,-0.150000000000001,
-10.0055609537896));
#32264=CARTESIAN_POINT('Ctrl Pts',(-5.8611219075793,-0.0750000000000014,
-14.15));
#32265=CARTESIAN_POINT('Ctrl Pts',(-1.7328752207935E-15,-1.51788304147971E-15,
-14.15));
#32266=CARTESIAN_POINT('Ctrl Pts',(5.86112190757929,0.0749999999999984,
-14.15));
#32267=CARTESIAN_POINT('Ctrl Pts',(10.0055609537896,0.149999999999998,-10.0055609537896));
#32268=CARTESIAN_POINT('Ctrl Pts',(14.15,0.224999999999998,-5.8611219075793));
#32269=CARTESIAN_POINT('Ctrl Pts',(14.15,0.299999999999998,-2.59931283119026E-15));
#32270=CARTESIAN_POINT('Ctrl Pts',(14.15,0.374999999999998,5.8611219075793));
#32271=CARTESIAN_POINT('Ctrl Pts',(10.0055609537896,0.449999999999997,10.0055609537896));
#32272=CARTESIAN_POINT('Ctrl Pts',(5.8611219075793,0.524999999999997,14.15));
#32273=CARTESIAN_POINT('Ctrl Pts',(0.,0.599999999999997,14.15));
#32274=CARTESIAN_POINT('Ctrl Pts',(-5.8611219075793,0.674999999999997,14.15));
#32275=CARTESIAN_POINT('Ctrl Pts',(-10.0055609537896,0.749999999999997,
10.0055609537896));
#32276=CARTESIAN_POINT('Ctrl Pts',(-14.15,0.824999999999997,5.8611219075793));
#32277=CARTESIAN_POINT('Ctrl Pts',(-14.15,0.899999999999996,8.66437610396752E-16));
#32278=CARTESIAN_POINT('Ctrl Pts',(-14.15,0.974999999999996,-5.86112190757929));
#32279=CARTESIAN_POINT('Ctrl Pts',(-10.0055609537896,1.05,-10.0055609537896));
#32280=CARTESIAN_POINT('Ctrl Pts',(-5.8611219075793,1.125,-14.15));
#32281=CARTESIAN_POINT('Ctrl Pts',(-1.7328752207935E-15,1.2,-14.15));
#32282=CARTESIAN_POINT('Ctrl Pts',(5.86112190757929,1.275,-14.15));
#32283=CARTESIAN_POINT('Ctrl Pts',(10.0055609537896,1.35,-10.0055609537896));
#32284=CARTESIAN_POINT('Ctrl Pts',(14.15,1.425,-5.8611219075793));
#32285=CARTESIAN_POINT('Ctrl Pts',(14.15,1.49999999999999,-2.59931283119026E-15));
#32286=CARTESIAN_POINT('Ctrl Pts',(14.15,1.57499999999999,5.8611219075793));
#32287=CARTESIAN_POINT('Ctrl Pts',(10.0055609537896,1.64999999999999,10.0055609537896));
#32288=CARTESIAN_POINT('Ctrl Pts',(5.8611219075793,1.72499999999999,14.15));
#32289=CARTESIAN_POINT('Ctrl Pts',(0.,1.79999999999999,14.15));
#32290=CARTESIAN_POINT('Ctrl Pts',(-5.8611219075793,1.87499999999999,14.15));
#32291=CARTESIAN_POINT('Ctrl Pts',(-10.0055609537896,1.94999999999999,10.0055609537896));
#32292=CARTESIAN_POINT('Ctrl Pts',(-14.15,2.02499999999999,5.8611219075793));
#32293=CARTESIAN_POINT('Ctrl Pts',(-14.15,2.09999999999999,8.66437610396752E-16));
#32294=CARTESIAN_POINT('Ctrl Pts',(-14.15,2.17499999999999,-5.86112190757929));
#32295=CARTESIAN_POINT('Ctrl Pts',(-10.0055609537896,2.24999999999999,-10.0055609537896));
#32296=CARTESIAN_POINT('Ctrl Pts',(-5.8611219075793,2.32499999999999,-14.15));
#32297=CARTESIAN_POINT('Ctrl Pts',(-1.7328752207935E-15,2.39999999999999,
-14.15));
#32298=CARTESIAN_POINT('Ctrl Pts',(5.86112190757929,2.47499999999999,-14.15));
#32299=CARTESIAN_POINT('Ctrl Pts',(10.0055609537896,2.54999999999999,-10.0055609537896));
#32300=CARTESIAN_POINT('Ctrl Pts',(14.15,2.62499999999999,-5.8611219075793));
#32301=CARTESIAN_POINT('Ctrl Pts',(14.15,2.69999999999999,-2.59931283119026E-15));
#32302=CARTESIAN_POINT('Ctrl Pts',(14.15,2.77499999999999,5.8611219075793));
#32303=CARTESIAN_POINT('Ctrl Pts',(10.0055609537896,2.84999999999999,10.0055609537896));
#32304=CARTESIAN_POINT('Ctrl Pts',(5.8611219075793,2.92499999999999,14.15));
#32305=CARTESIAN_POINT('Ctrl Pts',(0.,2.99999999999999,14.15));
#32306=CARTESIAN_POINT('Ctrl Pts',(-5.8611219075793,3.07499999999999,14.15));
#32307=CARTESIAN_POINT('Ctrl Pts',(-10.0055609537896,3.14999999999999,10.0055609537896));
#32308=CARTESIAN_POINT('Ctrl Pts',(-14.15,3.22499999999999,5.8611219075793));
#32309=CARTESIAN_POINT('Ctrl Pts',(-14.15,3.29999999999999,8.66437610396752E-16));
#32310=CARTESIAN_POINT('Ctrl Pts',(-14.15,3.37499999999999,-5.86112190757929));
#32311=CARTESIAN_POINT('Ctrl Pts',(-10.0055609537896,3.44999999999999,-10.0055609537896));
#32312=CARTESIAN_POINT('Ctrl Pts',(-5.8611219075793,3.52499999999999,-14.15));
#32313=CARTESIAN_POINT('Ctrl Pts',(-1.7328752207935E-15,3.59999999999999,
-14.15));
#32314=CARTESIAN_POINT('Ctrl Pts',(5.86112190757929,3.67499999999999,-14.15));
#32315=CARTESIAN_POINT('Ctrl Pts',(10.0055609537896,3.74999999999999,-10.0055609537896));
#32316=CARTESIAN_POINT('Ctrl Pts',(14.15,3.82499999999999,-5.8611219075793));
#32317=CARTESIAN_POINT('Ctrl Pts',(14.15,3.89999999999999,-2.59931283119026E-15));
#32318=CARTESIAN_POINT('Ctrl Pts',(14.15,3.97499999999999,5.8611219075793));
#32319=CARTESIAN_POINT('Ctrl Pts',(10.0055609537896,4.04999999999999,10.0055609537896));
#32320=CARTESIAN_POINT('Ctrl Pts',(5.8611219075793,4.12499999999999,14.15));
#32321=CARTESIAN_POINT('Ctrl Pts',(0.,4.19999999999999,14.15));
#32322=CARTESIAN_POINT('',(0.,7.34788079488412E-17,14.75));
#32323=CARTESIAN_POINT('Origin',(0.,0.,14.15));
#32324=CARTESIAN_POINT('',(-4.0476938186852E-13,4.79999999999999,14.75));
#32325=CARTESIAN_POINT('Ctrl Pts',(0.,7.34788079488412E-17,14.75));
#32326=CARTESIAN_POINT('Ctrl Pts',(-6.10965004500315,0.0749999999999999,
14.75));
#32327=CARTESIAN_POINT('Ctrl Pts',(-10.4298250225016,0.15,10.4298250225016));
#32328=CARTESIAN_POINT('Ctrl Pts',(-14.75,0.225,6.10965004500315));
#32329=CARTESIAN_POINT('Ctrl Pts',(-14.75,0.299999999999999,9.03177014371173E-16));
#32330=CARTESIAN_POINT('Ctrl Pts',(-14.75,0.374999999999999,-6.10965004500315));
#32331=CARTESIAN_POINT('Ctrl Pts',(-10.4298250225016,0.449999999999999,
-10.4298250225016));
#32332=CARTESIAN_POINT('Ctrl Pts',(-6.10965004500315,0.524999999999999,
-14.75));
#32333=CARTESIAN_POINT('Ctrl Pts',(-1.80635402874235E-15,0.599999999999999,
-14.75));
#32334=CARTESIAN_POINT('Ctrl Pts',(6.10965004500315,0.674999999999999,-14.75));
#32335=CARTESIAN_POINT('Ctrl Pts',(10.4298250225016,0.749999999999998,-10.4298250225016));
#32336=CARTESIAN_POINT('Ctrl Pts',(14.75,0.824999999999999,-6.10965004500316));
#32337=CARTESIAN_POINT('Ctrl Pts',(14.75,0.899999999999998,-2.70953104311352E-15));
#32338=CARTESIAN_POINT('Ctrl Pts',(14.75,0.974999999999998,6.10965004500316));
#32339=CARTESIAN_POINT('Ctrl Pts',(10.4298250225016,1.05,10.4298250225016));
#32340=CARTESIAN_POINT('Ctrl Pts',(6.10965004500316,1.125,14.75));
#32341=CARTESIAN_POINT('Ctrl Pts',(3.61270805748469E-15,1.2,14.75));
#32342=CARTESIAN_POINT('Ctrl Pts',(-6.10965004500315,1.275,14.75));
#32343=CARTESIAN_POINT('Ctrl Pts',(-10.4298250225016,1.35,10.4298250225016));
#32344=CARTESIAN_POINT('Ctrl Pts',(-14.75,1.425,6.10965004500316));
#32345=CARTESIAN_POINT('Ctrl Pts',(-14.75,1.5,4.51588507185587E-15));
#32346=CARTESIAN_POINT('Ctrl Pts',(-14.75,1.575,-6.10965004500315));
#32347=CARTESIAN_POINT('Ctrl Pts',(-10.4298250225016,1.65,-10.4298250225016));
#32348=CARTESIAN_POINT('Ctrl Pts',(-6.10965004500316,1.725,-14.75));
#32349=CARTESIAN_POINT('Ctrl Pts',(-5.41906208622704E-15,1.8,-14.75));
#32350=CARTESIAN_POINT('Ctrl Pts',(6.10965004500315,1.875,-14.75));
#32351=CARTESIAN_POINT('Ctrl Pts',(10.4298250225016,1.95,-10.4298250225016));
#32352=CARTESIAN_POINT('Ctrl Pts',(14.75,2.025,-6.10965004500317));
#32353=CARTESIAN_POINT('Ctrl Pts',(14.75,2.1,-6.32223910059821E-15));
#32354=CARTESIAN_POINT('Ctrl Pts',(14.75,2.17499999999999,6.10965004500315));
#32355=CARTESIAN_POINT('Ctrl Pts',(10.4298250225016,2.25,10.4298250225016));
#32356=CARTESIAN_POINT('Ctrl Pts',(6.10965004500317,2.32499999999999,14.75));
#32357=CARTESIAN_POINT('Ctrl Pts',(7.22541611496938E-15,2.39999999999999,
14.75));
#32358=CARTESIAN_POINT('Ctrl Pts',(-6.10965004500315,2.475,14.75));
#32359=CARTESIAN_POINT('Ctrl Pts',(-10.4298250225016,2.54999999999999,10.4298250225016));
#32360=CARTESIAN_POINT('Ctrl Pts',(-14.75,2.62499999999999,6.10965004500317));
#32361=CARTESIAN_POINT('Ctrl Pts',(-14.75,2.69999999999999,8.12859312934056E-15));
#32362=CARTESIAN_POINT('Ctrl Pts',(-14.75,2.77499999999999,-6.10965004500315));
#32363=CARTESIAN_POINT('Ctrl Pts',(-10.4298250225016,2.84999999999999,-10.4298250225016));
#32364=CARTESIAN_POINT('Ctrl Pts',(-6.10965004500317,2.92499999999999,-14.75));
#32365=CARTESIAN_POINT('Ctrl Pts',(-9.03177014371173E-15,2.99999999999999,
-14.75));
#32366=CARTESIAN_POINT('Ctrl Pts',(6.10965004500312,3.07499999999999,-14.75));
#32367=CARTESIAN_POINT('Ctrl Pts',(10.4298250225016,3.14999999999999,-10.4298250225016));
#32368=CARTESIAN_POINT('Ctrl Pts',(14.75,3.22499999999999,-6.10965004500317));
#32369=CARTESIAN_POINT('Ctrl Pts',(14.75,3.29999999999999,-3.61362105392366E-14));
#32370=CARTESIAN_POINT('Ctrl Pts',(14.75,3.37499999999999,6.10965004500315));
#32371=CARTESIAN_POINT('Ctrl Pts',(10.4298250225016,3.44999999999999,10.4298250225016));
#32372=CARTESIAN_POINT('Ctrl Pts',(6.10965004500314,3.52499999999999,14.75));
#32373=CARTESIAN_POINT('Ctrl Pts',(1.08381241724541E-14,3.59999999999999,
14.75));
#32374=CARTESIAN_POINT('Ctrl Pts',(-6.10965004500312,3.67499999999999,14.75));
#32375=CARTESIAN_POINT('Ctrl Pts',(-10.4298250225016,3.74999999999999,10.4298250225016));
#32376=CARTESIAN_POINT('Ctrl Pts',(-14.75,3.82499999999999,6.10965004500317));
#32377=CARTESIAN_POINT('Ctrl Pts',(-14.75,3.89999999999999,-1.44599621943284E-14));
#32378=CARTESIAN_POINT('Ctrl Pts',(-14.75,3.97499999999999,-6.10965004500315));
#32379=CARTESIAN_POINT('Ctrl Pts',(-10.4298250225016,4.04999999999999,-10.4298250225016));
#32380=CARTESIAN_POINT('Ctrl Pts',(-6.10965004500315,4.12499999999999,-14.75));
#32381=CARTESIAN_POINT('Ctrl Pts',(-1.26444782011964E-14,4.19999999999999,
-14.75));
#32382=CARTESIAN_POINT('Ctrl Pts',(6.10965004500312,4.27499999999999,-14.75));
#32383=CARTESIAN_POINT('Ctrl Pts',(10.4298250225016,4.34999999999999,-10.4298250225016));
#32384=CARTESIAN_POINT('Ctrl Pts',(14.75,4.42499999999999,-6.10965004500317));
#32385=CARTESIAN_POINT('Ctrl Pts',(14.75,4.49999999999999,-3.97489185967213E-14));
#32386=CARTESIAN_POINT('Ctrl Pts',(14.75,4.57499999999999,6.10965004500315));
#32387=CARTESIAN_POINT('Ctrl Pts',(10.4298250225016,4.64999999999999,10.4298250225016));
#32388=CARTESIAN_POINT('Ctrl Pts',(6.10965004500315,4.72499999999999,14.75));
#32389=CARTESIAN_POINT('Ctrl Pts',(-4.0476938186852E-13,4.79999999999999,
14.75));
#32390=CARTESIAN_POINT('Origin',(-7.90471375114085E-13,4.8,14.15));
#32391=CARTESIAN_POINT('Ctrl Pts',(0.,0.6,14.15));
#32392=CARTESIAN_POINT('Ctrl Pts',(-5.8611219075793,0.675,14.15));
#32393=CARTESIAN_POINT('Ctrl Pts',(-10.0055609537896,0.75,10.0055609537896));
#32394=CARTESIAN_POINT('Ctrl Pts',(-14.15,0.825,5.8611219075793));
#32395=CARTESIAN_POINT('Ctrl Pts',(-14.15,0.9,8.66437610396752E-16));
#32396=CARTESIAN_POINT('Ctrl Pts',(-14.15,0.974999999999999,-5.86112190757929));
#32397=CARTESIAN_POINT('Ctrl Pts',(-10.0055609537896,1.05,-10.0055609537896));
#32398=CARTESIAN_POINT('Ctrl Pts',(-5.8611219075793,1.125,-14.15));
#32399=CARTESIAN_POINT('Ctrl Pts',(-1.7328752207935E-15,1.2,-14.15));
#32400=CARTESIAN_POINT('Ctrl Pts',(5.86112190757929,1.275,-14.15));
#32401=CARTESIAN_POINT('Ctrl Pts',(10.0055609537896,1.35,-10.0055609537896));
#32402=CARTESIAN_POINT('Ctrl Pts',(14.15,1.425,-5.8611219075793));
#32403=CARTESIAN_POINT('Ctrl Pts',(14.15,1.5,-2.59931283119026E-15));
#32404=CARTESIAN_POINT('Ctrl Pts',(14.15,1.575,5.8611219075793));
#32405=CARTESIAN_POINT('Ctrl Pts',(10.0055609537896,1.65,10.0055609537896));
#32406=CARTESIAN_POINT('Ctrl Pts',(5.8611219075793,1.725,14.15));
#32407=CARTESIAN_POINT('Ctrl Pts',(0.,1.8,14.15));
#32408=CARTESIAN_POINT('Ctrl Pts',(-5.8611219075793,1.875,14.15));
#32409=CARTESIAN_POINT('Ctrl Pts',(-10.0055609537896,1.95,10.0055609537896));
#32410=CARTESIAN_POINT('Ctrl Pts',(-14.15,2.025,5.8611219075793));
#32411=CARTESIAN_POINT('Ctrl Pts',(-14.15,2.1,8.66437610396752E-16));
#32412=CARTESIAN_POINT('Ctrl Pts',(-14.15,2.175,-5.86112190757929));
#32413=CARTESIAN_POINT('Ctrl Pts',(-10.0055609537896,2.25,-10.0055609537896));
#32414=CARTESIAN_POINT('Ctrl Pts',(-5.8611219075793,2.325,-14.15));
#32415=CARTESIAN_POINT('Ctrl Pts',(-1.7328752207935E-15,2.4,-14.15));
#32416=CARTESIAN_POINT('Ctrl Pts',(5.86112190757929,2.475,-14.15));
#32417=CARTESIAN_POINT('Ctrl Pts',(10.0055609537896,2.55,-10.0055609537896));
#32418=CARTESIAN_POINT('Ctrl Pts',(14.15,2.625,-5.8611219075793));
#32419=CARTESIAN_POINT('Ctrl Pts',(14.15,2.7,-2.59931283119026E-15));
#32420=CARTESIAN_POINT('Ctrl Pts',(14.15,2.775,5.8611219075793));
#32421=CARTESIAN_POINT('Ctrl Pts',(10.0055609537896,2.85,10.0055609537896));
#32422=CARTESIAN_POINT('Ctrl Pts',(5.8611219075793,2.92499999999999,14.15));
#32423=CARTESIAN_POINT('Ctrl Pts',(0.,2.99999999999999,14.15));
#32424=CARTESIAN_POINT('Ctrl Pts',(-5.8611219075793,3.07499999999999,14.15));
#32425=CARTESIAN_POINT('Ctrl Pts',(-10.0055609537896,3.15,10.0055609537896));
#32426=CARTESIAN_POINT('Ctrl Pts',(-14.15,3.22499999999999,5.8611219075793));
#32427=CARTESIAN_POINT('Ctrl Pts',(-14.15,3.29999999999999,8.66437610396752E-16));
#32428=CARTESIAN_POINT('Ctrl Pts',(-14.15,3.37499999999999,-5.86112190757929));
#32429=CARTESIAN_POINT('Ctrl Pts',(-10.0055609537896,3.44999999999999,-10.0055609537896));
#32430=CARTESIAN_POINT('Ctrl Pts',(-5.8611219075793,3.52499999999999,-14.15));
#32431=CARTESIAN_POINT('Ctrl Pts',(-1.7328752207935E-15,3.59999999999999,
-14.15));
#32432=CARTESIAN_POINT('Ctrl Pts',(5.86112190757929,3.67499999999999,-14.15));
#32433=CARTESIAN_POINT('Ctrl Pts',(10.0055609537896,3.74999999999999,-10.0055609537896));
#32434=CARTESIAN_POINT('Ctrl Pts',(14.15,3.82499999999999,-5.8611219075793));
#32435=CARTESIAN_POINT('Ctrl Pts',(14.15,3.89999999999999,-2.59931283119026E-15));
#32436=CARTESIAN_POINT('Ctrl Pts',(14.15,3.97499999999999,5.8611219075793));
#32437=CARTESIAN_POINT('Ctrl Pts',(10.0055609537896,4.04999999999999,10.0055609537896));
#32438=CARTESIAN_POINT('Ctrl Pts',(5.8611219075793,4.12499999999999,14.15));
#32439=CARTESIAN_POINT('Ctrl Pts',(0.,4.19999999999999,14.15));
#32440=CARTESIAN_POINT('Ctrl Pts',(-5.8611219075793,4.27499999999999,14.15));
#32441=CARTESIAN_POINT('Ctrl Pts',(-10.0055609537896,4.34999999999999,10.0055609537896));
#32442=CARTESIAN_POINT('Ctrl Pts',(-14.15,4.42499999999999,5.8611219075793));
#32443=CARTESIAN_POINT('Ctrl Pts',(-14.15,4.49999999999999,8.66437610396752E-16));
#32444=CARTESIAN_POINT('Ctrl Pts',(-14.15,4.57499999999999,-5.86112190757929));
#32445=CARTESIAN_POINT('Ctrl Pts',(-10.0055609537896,4.64999999999999,-10.0055609537896));
#32446=CARTESIAN_POINT('Ctrl Pts',(-5.8611219075793,4.72499999999999,-14.15));
#32447=CARTESIAN_POINT('Ctrl Pts',(-1.7328752207935E-15,4.79999999999999,
-14.15));
#32448=CARTESIAN_POINT('Ctrl Pts',(5.86112190757929,4.87499999999999,-14.15));
#32449=CARTESIAN_POINT('Ctrl Pts',(10.0055609537896,4.94999999999999,-10.0055609537896));
#32450=CARTESIAN_POINT('Ctrl Pts',(14.15,5.02499999999999,-5.8611219075793));
#32451=CARTESIAN_POINT('Ctrl Pts',(14.15,5.09999999999999,-2.59931283119026E-15));
#32452=CARTESIAN_POINT('Ctrl Pts',(14.15,5.17499999999999,5.8611219075793));
#32453=CARTESIAN_POINT('Ctrl Pts',(10.0055609537896,5.24999999999999,10.0055609537896));
#32454=CARTESIAN_POINT('Ctrl Pts',(5.8611219075793,5.32499999999999,14.15));
#32455=CARTESIAN_POINT('Ctrl Pts',(0.,5.39999999999999,14.15));
#32456=CARTESIAN_POINT('Ctrl Pts',(0.,0.6,14.5014718625761));
#32457=CARTESIAN_POINT('Ctrl Pts',(-6.00670631985087,0.675,14.5014718625761));
#32458=CARTESIAN_POINT('Ctrl Pts',(-10.2540890912135,0.75,10.2540890912135));
#32459=CARTESIAN_POINT('Ctrl Pts',(-14.5014718625761,0.825,6.00670631985087));
#32460=CARTESIAN_POINT('Ctrl Pts',(-14.5014718625761,0.9,8.87959054971464E-16));
#32461=CARTESIAN_POINT('Ctrl Pts',(-14.5014718625761,0.974999999999999,
-6.00670631985087));
#32462=CARTESIAN_POINT('Ctrl Pts',(-10.2540890912135,1.05,-10.2540890912135));
#32463=CARTESIAN_POINT('Ctrl Pts',(-6.00670631985087,1.125,-14.5014718625761));
#32464=CARTESIAN_POINT('Ctrl Pts',(-1.77591810994293E-15,1.2,-14.5014718625761));
#32465=CARTESIAN_POINT('Ctrl Pts',(6.00670631985087,1.275,-14.5014718625761));
#32466=CARTESIAN_POINT('Ctrl Pts',(10.2540890912135,1.35,-10.2540890912135));
#32467=CARTESIAN_POINT('Ctrl Pts',(14.5014718625761,1.425,-6.00670631985087));
#32468=CARTESIAN_POINT('Ctrl Pts',(14.5014718625761,1.5,-2.66387716491439E-15));
#32469=CARTESIAN_POINT('Ctrl Pts',(14.5014718625761,1.575,6.00670631985087));
#32470=CARTESIAN_POINT('Ctrl Pts',(10.2540890912135,1.65,10.2540890912135));
#32471=CARTESIAN_POINT('Ctrl Pts',(6.00670631985088,1.725,14.5014718625761));
#32472=CARTESIAN_POINT('Ctrl Pts',(0.,1.8,14.5014718625761));
#32473=CARTESIAN_POINT('Ctrl Pts',(-6.00670631985087,1.875,14.5014718625761));
#32474=CARTESIAN_POINT('Ctrl Pts',(-10.2540890912135,1.95,10.2540890912135));
#32475=CARTESIAN_POINT('Ctrl Pts',(-14.5014718625761,2.025,6.00670631985087));
#32476=CARTESIAN_POINT('Ctrl Pts',(-14.5014718625761,2.1,8.87959054971464E-16));
#32477=CARTESIAN_POINT('Ctrl Pts',(-14.5014718625761,2.175,-6.00670631985087));
#32478=CARTESIAN_POINT('Ctrl Pts',(-10.2540890912135,2.25,-10.2540890912135));
#32479=CARTESIAN_POINT('Ctrl Pts',(-6.00670631985087,2.325,-14.5014718625761));
#32480=CARTESIAN_POINT('Ctrl Pts',(-1.77591810994293E-15,2.4,-14.5014718625761));
#32481=CARTESIAN_POINT('Ctrl Pts',(6.00670631985087,2.475,-14.5014718625761));
#32482=CARTESIAN_POINT('Ctrl Pts',(10.2540890912135,2.55,-10.2540890912135));
#32483=CARTESIAN_POINT('Ctrl Pts',(14.5014718625761,2.625,-6.00670631985087));
#32484=CARTESIAN_POINT('Ctrl Pts',(14.5014718625761,2.7,-2.66387716491439E-15));
#32485=CARTESIAN_POINT('Ctrl Pts',(14.5014718625761,2.775,6.00670631985087));
#32486=CARTESIAN_POINT('Ctrl Pts',(10.2540890912135,2.85,10.2540890912135));
#32487=CARTESIAN_POINT('Ctrl Pts',(6.00670631985088,2.92499999999999,14.5014718625761));
#32488=CARTESIAN_POINT('Ctrl Pts',(0.,2.99999999999999,14.5014718625761));
#32489=CARTESIAN_POINT('Ctrl Pts',(-6.00670631985087,3.075,14.5014718625761));
#32490=CARTESIAN_POINT('Ctrl Pts',(-10.2540890912135,3.14999999999999,10.2540890912135));
#32491=CARTESIAN_POINT('Ctrl Pts',(-14.5014718625761,3.22499999999999,6.00670631985087));
#32492=CARTESIAN_POINT('Ctrl Pts',(-14.5014718625761,3.29999999999999,8.87959054971464E-16));
#32493=CARTESIAN_POINT('Ctrl Pts',(-14.5014718625761,3.37499999999999,-6.00670631985087));
#32494=CARTESIAN_POINT('Ctrl Pts',(-10.2540890912135,3.44999999999999,-10.2540890912135));
#32495=CARTESIAN_POINT('Ctrl Pts',(-6.00670631985087,3.52499999999999,-14.5014718625761));
#32496=CARTESIAN_POINT('Ctrl Pts',(-1.77591810994293E-15,3.59999999999999,
-14.5014718625761));
#32497=CARTESIAN_POINT('Ctrl Pts',(6.00670631985087,3.67499999999999,-14.5014718625761));
#32498=CARTESIAN_POINT('Ctrl Pts',(10.2540890912135,3.74999999999999,-10.2540890912135));
#32499=CARTESIAN_POINT('Ctrl Pts',(14.5014718625761,3.82499999999999,-6.00670631985087));
#32500=CARTESIAN_POINT('Ctrl Pts',(14.5014718625761,3.89999999999999,-2.66387716491439E-15));
#32501=CARTESIAN_POINT('Ctrl Pts',(14.5014718625761,3.97499999999999,6.00670631985087));
#32502=CARTESIAN_POINT('Ctrl Pts',(10.2540890912135,4.04999999999999,10.2540890912135));
#32503=CARTESIAN_POINT('Ctrl Pts',(6.00670631985088,4.12499999999999,14.5014718625761));
#32504=CARTESIAN_POINT('Ctrl Pts',(0.,4.19999999999999,14.5014718625761));
#32505=CARTESIAN_POINT('Ctrl Pts',(-6.00670631985087,4.27499999999999,14.5014718625761));
#32506=CARTESIAN_POINT('Ctrl Pts',(-10.2540890912135,4.34999999999999,10.2540890912135));
#32507=CARTESIAN_POINT('Ctrl Pts',(-14.5014718625761,4.42499999999999,6.00670631985087));
#32508=CARTESIAN_POINT('Ctrl Pts',(-14.5014718625761,4.49999999999999,8.87959054971464E-16));
#32509=CARTESIAN_POINT('Ctrl Pts',(-14.5014718625761,4.57499999999999,-6.00670631985087));
#32510=CARTESIAN_POINT('Ctrl Pts',(-10.2540890912135,4.64999999999999,-10.2540890912135));
#32511=CARTESIAN_POINT('Ctrl Pts',(-6.00670631985087,4.72499999999999,-14.5014718625761));
#32512=CARTESIAN_POINT('Ctrl Pts',(-1.77591810994293E-15,4.79999999999999,
-14.5014718625761));
#32513=CARTESIAN_POINT('Ctrl Pts',(6.00670631985087,4.87499999999999,-14.5014718625761));
#32514=CARTESIAN_POINT('Ctrl Pts',(10.2540890912135,4.94999999999999,-10.2540890912135));
#32515=CARTESIAN_POINT('Ctrl Pts',(14.5014718625761,5.02499999999999,-6.00670631985087));
#32516=CARTESIAN_POINT('Ctrl Pts',(14.5014718625761,5.09999999999999,-2.66387716491439E-15));
#32517=CARTESIAN_POINT('Ctrl Pts',(14.5014718625761,5.17499999999999,6.00670631985087));
#32518=CARTESIAN_POINT('Ctrl Pts',(10.2540890912135,5.24999999999999,10.2540890912135));
#32519=CARTESIAN_POINT('Ctrl Pts',(6.00670631985088,5.32499999999999,14.5014718625761));
#32520=CARTESIAN_POINT('Ctrl Pts',(0.,5.39999999999999,14.5014718625761));
#32521=CARTESIAN_POINT('Ctrl Pts',(0.,0.351471862576143,14.75));
#32522=CARTESIAN_POINT('Ctrl Pts',(-6.10965004500315,0.426471862576143,
14.75));
#32523=CARTESIAN_POINT('Ctrl Pts',(-10.4298250225016,0.501471862576143,
10.4298250225016));
#32524=CARTESIAN_POINT('Ctrl Pts',(-14.75,0.576471862576143,6.10965004500315));
#32525=CARTESIAN_POINT('Ctrl Pts',(-14.75,0.651471862576142,9.03177014371173E-16));
#32526=CARTESIAN_POINT('Ctrl Pts',(-14.75,0.726471862576142,-6.10965004500315));
#32527=CARTESIAN_POINT('Ctrl Pts',(-10.4298250225016,0.801471862576142,
-10.4298250225016));
#32528=CARTESIAN_POINT('Ctrl Pts',(-6.10965004500315,0.876471862576142,
-14.75));
#32529=CARTESIAN_POINT('Ctrl Pts',(-1.80635402874235E-15,0.951471862576142,
-14.75));
#32530=CARTESIAN_POINT('Ctrl Pts',(6.10965004500315,1.02647186257614,-14.75));
#32531=CARTESIAN_POINT('Ctrl Pts',(10.4298250225016,1.10147186257614,-10.4298250225016));
#32532=CARTESIAN_POINT('Ctrl Pts',(14.75,1.17647186257614,-6.10965004500316));
#32533=CARTESIAN_POINT('Ctrl Pts',(14.75,1.25147186257614,-2.70953104311352E-15));
#32534=CARTESIAN_POINT('Ctrl Pts',(14.75,1.32647186257614,6.10965004500316));
#32535=CARTESIAN_POINT('Ctrl Pts',(10.4298250225016,1.40147186257614,10.4298250225016));
#32536=CARTESIAN_POINT('Ctrl Pts',(6.10965004500316,1.47647186257614,14.75));
#32537=CARTESIAN_POINT('Ctrl Pts',(0.,1.55147186257614,14.75));
#32538=CARTESIAN_POINT('Ctrl Pts',(-6.10965004500315,1.62647186257614,14.75));
#32539=CARTESIAN_POINT('Ctrl Pts',(-10.4298250225016,1.70147186257614,10.4298250225016));
#32540=CARTESIAN_POINT('Ctrl Pts',(-14.75,1.77647186257614,6.10965004500315));
#32541=CARTESIAN_POINT('Ctrl Pts',(-14.75,1.85147186257614,9.03177014371173E-16));
#32542=CARTESIAN_POINT('Ctrl Pts',(-14.75,1.92647186257614,-6.10965004500315));
#32543=CARTESIAN_POINT('Ctrl Pts',(-10.4298250225016,2.00147186257614,-10.4298250225016));
#32544=CARTESIAN_POINT('Ctrl Pts',(-6.10965004500315,2.07647186257614,-14.75));
#32545=CARTESIAN_POINT('Ctrl Pts',(-1.80635402874235E-15,2.15147186257614,
-14.75));
#32546=CARTESIAN_POINT('Ctrl Pts',(6.10965004500315,2.22647186257614,-14.75));
#32547=CARTESIAN_POINT('Ctrl Pts',(10.4298250225016,2.30147186257614,-10.4298250225016));
#32548=CARTESIAN_POINT('Ctrl Pts',(14.75,2.37647186257614,-6.10965004500316));
#32549=CARTESIAN_POINT('Ctrl Pts',(14.75,2.45147186257614,-2.70953104311352E-15));
#32550=CARTESIAN_POINT('Ctrl Pts',(14.75,2.52647186257614,6.10965004500316));
#32551=CARTESIAN_POINT('Ctrl Pts',(10.4298250225016,2.60147186257614,10.4298250225016));
#32552=CARTESIAN_POINT('Ctrl Pts',(6.10965004500316,2.67647186257614,14.75));
#32553=CARTESIAN_POINT('Ctrl Pts',(0.,2.75147186257614,14.75));
#32554=CARTESIAN_POINT('Ctrl Pts',(-6.10965004500315,2.82647186257614,14.75));
#32555=CARTESIAN_POINT('Ctrl Pts',(-10.4298250225016,2.90147186257614,10.4298250225016));
#32556=CARTESIAN_POINT('Ctrl Pts',(-14.75,2.97647186257614,6.10965004500315));
#32557=CARTESIAN_POINT('Ctrl Pts',(-14.75,3.05147186257614,9.03177014371173E-16));
#32558=CARTESIAN_POINT('Ctrl Pts',(-14.75,3.12647186257614,-6.10965004500315));
#32559=CARTESIAN_POINT('Ctrl Pts',(-10.4298250225016,3.20147186257614,-10.4298250225016));
#32560=CARTESIAN_POINT('Ctrl Pts',(-6.10965004500315,3.27647186257614,-14.75));
#32561=CARTESIAN_POINT('Ctrl Pts',(-1.80635402874235E-15,3.35147186257614,
-14.75));
#32562=CARTESIAN_POINT('Ctrl Pts',(6.10965004500315,3.42647186257614,-14.75));
#32563=CARTESIAN_POINT('Ctrl Pts',(10.4298250225016,3.50147186257614,-10.4298250225016));
#32564=CARTESIAN_POINT('Ctrl Pts',(14.75,3.57647186257614,-6.10965004500316));
#32565=CARTESIAN_POINT('Ctrl Pts',(14.75,3.65147186257614,-2.70953104311352E-15));
#32566=CARTESIAN_POINT('Ctrl Pts',(14.75,3.72647186257614,6.10965004500316));
#32567=CARTESIAN_POINT('Ctrl Pts',(10.4298250225016,3.80147186257614,10.4298250225016));
#32568=CARTESIAN_POINT('Ctrl Pts',(6.10965004500316,3.87647186257614,14.75));
#32569=CARTESIAN_POINT('Ctrl Pts',(0.,3.95147186257614,14.75));
#32570=CARTESIAN_POINT('Ctrl Pts',(-6.10965004500315,4.02647186257614,14.75));
#32571=CARTESIAN_POINT('Ctrl Pts',(-10.4298250225016,4.10147186257613,10.4298250225016));
#32572=CARTESIAN_POINT('Ctrl Pts',(-14.75,4.17647186257613,6.10965004500315));
#32573=CARTESIAN_POINT('Ctrl Pts',(-14.75,4.25147186257614,9.03177014371173E-16));
#32574=CARTESIAN_POINT('Ctrl Pts',(-14.75,4.32647186257613,-6.10965004500315));
#32575=CARTESIAN_POINT('Ctrl Pts',(-10.4298250225016,4.40147186257613,-10.4298250225016));
#32576=CARTESIAN_POINT('Ctrl Pts',(-6.10965004500315,4.47647186257614,-14.75));
#32577=CARTESIAN_POINT('Ctrl Pts',(-1.80635402874235E-15,4.55147186257613,
-14.75));
#32578=CARTESIAN_POINT('Ctrl Pts',(6.10965004500315,4.62647186257613,-14.75));
#32579=CARTESIAN_POINT('Ctrl Pts',(10.4298250225016,4.70147186257613,-10.4298250225016));
#32580=CARTESIAN_POINT('Ctrl Pts',(14.75,4.77647186257613,-6.10965004500316));
#32581=CARTESIAN_POINT('Ctrl Pts',(14.75,4.85147186257613,-2.70953104311352E-15));
#32582=CARTESIAN_POINT('Ctrl Pts',(14.75,4.92647186257613,6.10965004500316));
#32583=CARTESIAN_POINT('Ctrl Pts',(10.4298250225016,5.00147186257613,10.4298250225016));
#32584=CARTESIAN_POINT('Ctrl Pts',(6.10965004500316,5.07647186257613,14.75));
#32585=CARTESIAN_POINT('Ctrl Pts',(0.,5.15147186257613,14.75));
#32586=CARTESIAN_POINT('Ctrl Pts',(0.,7.34788079488412E-17,14.75));
#32587=CARTESIAN_POINT('Ctrl Pts',(-6.10965004500315,0.0749999999999999,
14.75));
#32588=CARTESIAN_POINT('Ctrl Pts',(-10.4298250225016,0.15,10.4298250225016));
#32589=CARTESIAN_POINT('Ctrl Pts',(-14.75,0.225,6.10965004500315));
#32590=CARTESIAN_POINT('Ctrl Pts',(-14.75,0.299999999999999,9.03177014371173E-16));
#32591=CARTESIAN_POINT('Ctrl Pts',(-14.75,0.374999999999999,-6.10965004500315));
#32592=CARTESIAN_POINT('Ctrl Pts',(-10.4298250225016,0.449999999999999,
-10.4298250225016));
#32593=CARTESIAN_POINT('Ctrl Pts',(-6.10965004500315,0.524999999999999,
-14.75));
#32594=CARTESIAN_POINT('Ctrl Pts',(-1.80635402874235E-15,0.599999999999999,
-14.75));
#32595=CARTESIAN_POINT('Ctrl Pts',(6.10965004500315,0.674999999999999,-14.75));
#32596=CARTESIAN_POINT('Ctrl Pts',(10.4298250225016,0.749999999999998,-10.4298250225016));
#32597=CARTESIAN_POINT('Ctrl Pts',(14.75,0.824999999999999,-6.10965004500316));
#32598=CARTESIAN_POINT('Ctrl Pts',(14.75,0.899999999999998,-2.70953104311352E-15));
#32599=CARTESIAN_POINT('Ctrl Pts',(14.75,0.974999999999998,6.10965004500316));
#32600=CARTESIAN_POINT('Ctrl Pts',(10.4298250225016,1.05,10.4298250225016));
#32601=CARTESIAN_POINT('Ctrl Pts',(6.10965004500316,1.125,14.75));
#32602=CARTESIAN_POINT('Ctrl Pts',(0.,1.2,14.75));
#32603=CARTESIAN_POINT('Ctrl Pts',(-6.10965004500315,1.275,14.75));
#32604=CARTESIAN_POINT('Ctrl Pts',(-10.4298250225016,1.35,10.4298250225016));
#32605=CARTESIAN_POINT('Ctrl Pts',(-14.75,1.425,6.10965004500315));
#32606=CARTESIAN_POINT('Ctrl Pts',(-14.75,1.5,9.03177014371173E-16));
#32607=CARTESIAN_POINT('Ctrl Pts',(-14.75,1.575,-6.10965004500315));
#32608=CARTESIAN_POINT('Ctrl Pts',(-10.4298250225016,1.65,-10.4298250225016));
#32609=CARTESIAN_POINT('Ctrl Pts',(-6.10965004500315,1.725,-14.75));
#32610=CARTESIAN_POINT('Ctrl Pts',(-1.80635402874235E-15,1.8,-14.75));
#32611=CARTESIAN_POINT('Ctrl Pts',(6.10965004500315,1.875,-14.75));
#32612=CARTESIAN_POINT('Ctrl Pts',(10.4298250225016,1.95,-10.4298250225016));
#32613=CARTESIAN_POINT('Ctrl Pts',(14.75,2.025,-6.10965004500316));
#32614=CARTESIAN_POINT('Ctrl Pts',(14.75,2.1,-2.70953104311352E-15));
#32615=CARTESIAN_POINT('Ctrl Pts',(14.75,2.17499999999999,6.10965004500316));
#32616=CARTESIAN_POINT('Ctrl Pts',(10.4298250225016,2.25,10.4298250225016));
#32617=CARTESIAN_POINT('Ctrl Pts',(6.10965004500316,2.32499999999999,14.75));
#32618=CARTESIAN_POINT('Ctrl Pts',(0.,2.39999999999999,14.75));
#32619=CARTESIAN_POINT('Ctrl Pts',(-6.10965004500315,2.47499999999999,14.75));
#32620=CARTESIAN_POINT('Ctrl Pts',(-10.4298250225016,2.54999999999999,10.4298250225016));
#32621=CARTESIAN_POINT('Ctrl Pts',(-14.75,2.62499999999999,6.10965004500315));
#32622=CARTESIAN_POINT('Ctrl Pts',(-14.75,2.69999999999999,9.03177014371173E-16));
#32623=CARTESIAN_POINT('Ctrl Pts',(-14.75,2.77499999999999,-6.10965004500315));
#32624=CARTESIAN_POINT('Ctrl Pts',(-10.4298250225016,2.84999999999999,-10.4298250225016));
#32625=CARTESIAN_POINT('Ctrl Pts',(-6.10965004500315,2.92499999999999,-14.75));
#32626=CARTESIAN_POINT('Ctrl Pts',(-1.80635402874235E-15,2.99999999999999,
-14.75));
#32627=CARTESIAN_POINT('Ctrl Pts',(6.10965004500315,3.07499999999999,-14.75));
#32628=CARTESIAN_POINT('Ctrl Pts',(10.4298250225016,3.14999999999999,-10.4298250225016));
#32629=CARTESIAN_POINT('Ctrl Pts',(14.75,3.22499999999999,-6.10965004500316));
#32630=CARTESIAN_POINT('Ctrl Pts',(14.75,3.29999999999999,-2.70953104311352E-15));
#32631=CARTESIAN_POINT('Ctrl Pts',(14.75,3.37499999999999,6.10965004500316));
#32632=CARTESIAN_POINT('Ctrl Pts',(10.4298250225016,3.44999999999999,10.4298250225016));
#32633=CARTESIAN_POINT('Ctrl Pts',(6.10965004500316,3.52499999999999,14.75));
#32634=CARTESIAN_POINT('Ctrl Pts',(0.,3.59999999999999,14.75));
#32635=CARTESIAN_POINT('Ctrl Pts',(-6.10965004500315,3.67499999999999,14.75));
#32636=CARTESIAN_POINT('Ctrl Pts',(-10.4298250225016,3.74999999999999,10.4298250225016));
#32637=CARTESIAN_POINT('Ctrl Pts',(-14.75,3.82499999999999,6.10965004500315));
#32638=CARTESIAN_POINT('Ctrl Pts',(-14.75,3.89999999999999,9.03177014371173E-16));
#32639=CARTESIAN_POINT('Ctrl Pts',(-14.75,3.97499999999999,-6.10965004500315));
#32640=CARTESIAN_POINT('Ctrl Pts',(-10.4298250225016,4.04999999999999,-10.4298250225016));
#32641=CARTESIAN_POINT('Ctrl Pts',(-6.10965004500315,4.12499999999999,-14.75));
#32642=CARTESIAN_POINT('Ctrl Pts',(-1.80635402874235E-15,4.19999999999999,
-14.75));
#32643=CARTESIAN_POINT('Ctrl Pts',(6.10965004500315,4.27499999999999,-14.75));
#32644=CARTESIAN_POINT('Ctrl Pts',(10.4298250225016,4.34999999999999,-10.4298250225016));
#32645=CARTESIAN_POINT('Ctrl Pts',(14.75,4.42499999999999,-6.10965004500316));
#32646=CARTESIAN_POINT('Ctrl Pts',(14.75,4.49999999999999,-2.70953104311352E-15));
#32647=CARTESIAN_POINT('Ctrl Pts',(14.75,4.57499999999999,6.10965004500316));
#32648=CARTESIAN_POINT('Ctrl Pts',(10.4298250225016,4.64999999999999,10.4298250225016));
#32649=CARTESIAN_POINT('Ctrl Pts',(6.10965004500316,4.72499999999999,14.75));
#32650=CARTESIAN_POINT('Ctrl Pts',(0.,4.79999999999999,14.75));
#32651=CARTESIAN_POINT('Origin',(0.,0.,14.15));
#32652=CARTESIAN_POINT('Origin',(-7.90471375114085E-13,4.8,14.15));
#32653=CARTESIAN_POINT('Origin',(-7.90471375114085E-13,4.8,14.15));
#32654=CARTESIAN_POINT('Origin',(0.,0.,14.15));
#32655=CARTESIAN_POINT('',(0.,0.,0.));
#32656=CARTESIAN_POINT('Origin',(-16.1,-2.1492551325036E-15,0.));
#32657=CARTESIAN_POINT('',(-2.32682891837997E-15,-2.32682891837997E-15,
19.));
#32658=CARTESIAN_POINT('Origin',(0.,-2.32682891837997E-15,0.));
#32659=CARTESIAN_POINT('',(-1.97168134662724E-15,-1.97168134662724E-15,
16.1));
#32660=CARTESIAN_POINT('Origin',(0.,-1.97168134662724E-15,0.));
#32661=CARTESIAN_POINT('Origin',(0.,0.,0.));
#32662=CARTESIAN_POINT('',(-2.32682891837997E-15,14.,19.));
#32663=CARTESIAN_POINT('',(-2.32682891837997E-15,0.,19.));
#32664=CARTESIAN_POINT('Origin',(0.,14.,0.));
#32665=CARTESIAN_POINT('Origin',(0.,27.2849025449883,0.));
#32666=CARTESIAN_POINT('',(-2.0818995585505E-15,28.,17.));
#32667=CARTESIAN_POINT('Origin',(-7.59211428773629E-15,27.2849025449883,
61.9943178149179));
#32668=CARTESIAN_POINT('Origin',(0.,28.,0.));
#32669=CARTESIAN_POINT('Origin',(0.,32.,0.));
#32670=CARTESIAN_POINT('',(-1.95943487863577E-15,32.,16.));
#32671=CARTESIAN_POINT('',(-1.95943487863577E-15,32.,16.));
#32672=CARTESIAN_POINT('Origin',(0.,32.,0.));
#32673=CARTESIAN_POINT('Origin',(-16.,32.,0.));
#32674=CARTESIAN_POINT('',(-1.60428730688303E-15,32.,13.1));
#32675=CARTESIAN_POINT('Origin',(0.,32.,0.));
#32676=CARTESIAN_POINT('Origin',(0.,0.,0.));
#32677=CARTESIAN_POINT('',(-1.60428730688303E-15,29.5,13.1));
#32678=CARTESIAN_POINT('',(-1.60428730688303E-15,0.,13.1));
#32679=CARTESIAN_POINT('Origin',(0.,29.5,0.));
#32680=CARTESIAN_POINT('Origin',(-13.1,29.5,0.));
#32681=CARTESIAN_POINT('',(-1.8492166667125E-15,29.5,15.1));
#32682=CARTESIAN_POINT('Origin',(0.,29.5,0.));
#32683=CARTESIAN_POINT('Origin',(0.,0.,0.));
#32684=CARTESIAN_POINT('',(-1.8492166667125E-15,23.9,15.1));
#32685=CARTESIAN_POINT('',(-1.8492166667125E-15,0.,15.1));
#32686=CARTESIAN_POINT('',(0.,23.9,-15.1));
#32687=CARTESIAN_POINT('Origin',(0.,23.9,0.));
#32688=CARTESIAN_POINT('Origin',(0.,23.9,0.));
#32689=CARTESIAN_POINT('Origin',(0.,22.9,0.));
#32690=CARTESIAN_POINT('',(0.,22.9,-14.1));
#32691=CARTESIAN_POINT('',(-1.72675198679777E-15,22.9,14.1));
#32692=CARTESIAN_POINT('Origin',(0.,22.9,0.));
#32693=CARTESIAN_POINT('Origin',(0.,22.9,0.));
#32694=CARTESIAN_POINT('',(-1.72675198679777E-15,22.9,-14.1));
#32695=CARTESIAN_POINT('Origin',(0.,0.,0.));
#32696=CARTESIAN_POINT('',(-1.72675198679777E-15,18.9,14.1));
#32697=CARTESIAN_POINT('',(-1.72675198679777E-15,0.,14.1));
#32698=CARTESIAN_POINT('',(0.,18.9,-14.1));
#32699=CARTESIAN_POINT('Origin',(0.,18.9,0.));
#32700=CARTESIAN_POINT('Origin',(0.,18.9,0.));
#32701=CARTESIAN_POINT('Origin',(0.,17.9995959557022,0.));
#32702=CARTESIAN_POINT('',(0.,17.9995959557022,-13.1));
#32703=CARTESIAN_POINT('',(-1.60428730688303E-15,17.9995959557022,13.1));
#32704=CARTESIAN_POINT('Origin',(0.,17.9995959557022,0.));
#32705=CARTESIAN_POINT('Origin',(0.,17.9995959557022,0.));
#32706=CARTESIAN_POINT('',(-1.60428730688303E-15,17.9995959557022,-13.1));
#32707=CARTESIAN_POINT('Origin',(0.,0.,0.));
#32708=CARTESIAN_POINT('',(-1.60428730688303E-15,16.,13.1));
#32709=CARTESIAN_POINT('',(-1.60428730688303E-15,0.,13.1));
#32710=CARTESIAN_POINT('Origin',(0.,16.,0.));
#32711=CARTESIAN_POINT('Origin',(-13.1,16.,0.));
#32712=CARTESIAN_POINT('',(-1.97168134662724E-15,16.,16.1));
#32713=CARTESIAN_POINT('Origin',(0.,16.,0.));
#32714=CARTESIAN_POINT('Origin',(0.,0.,0.));
#32715=CARTESIAN_POINT('',(-1.97168134662724E-15,0.,16.1));
#32716=CARTESIAN_POINT('',(0.,0.,0.));
#32717=CARTESIAN_POINT('Origin',(0.,0.,0.));
#32718=CARTESIAN_POINT('',(-1.75,1.94289029309402E-16,-1.07156594925393E-16));
#32719=CARTESIAN_POINT('',(1.75,-1.94289029309402E-16,-1.07156594925393E-16));
#32720=CARTESIAN_POINT('Origin',(0.,0.,0.));
#32721=CARTESIAN_POINT('',(0.,0.,0.));
#32722=CARTESIAN_POINT('',(0.,0.,42.));
#32723=CARTESIAN_POINT('',(0.,-12.04,125.));
#32724=CARTESIAN_POINT('',(0.,0.,111.475));
#32725=CARTESIAN_POINT('',(0.,9.33720274436333E-18,105.599975054442));
#32726=CARTESIAN_POINT('',(11.4507204561937,-3.72056461227434,125.));
#32727=CARTESIAN_POINT('',(7.07693443760133,9.74056461227441,125.));
#32728=CARTESIAN_POINT('',(-7.07693443760147,9.74056461227431,125.));
#32729=CARTESIAN_POINT('',(-11.4507204561936,-3.7205646122745,125.));
#32730=CARTESIAN_POINT('',(0.,0.,0.));
#32731=CARTESIAN_POINT('Origin',(0.,15.5,0.));
#32732=CARTESIAN_POINT('',(-1.34711147906209E-15,15.5,11.));
#32733=CARTESIAN_POINT('Origin',(0.,15.5,0.));
#32734=CARTESIAN_POINT('Origin',(0.,15.5,0.));
#32735=CARTESIAN_POINT('',(-1.92881870865708E-15,14.5,15.75));
#32736=CARTESIAN_POINT('Origin',(0.,14.5,0.));
#32737=CARTESIAN_POINT('',(-1.34711147906209E-15,15.5,11.));
#32738=CARTESIAN_POINT('Origin',(0.,0.,0.));
#32739=CARTESIAN_POINT('',(0.,9.00000000000002,15.75));
#32740=CARTESIAN_POINT('',(-1.92881870865708E-15,9.00000000000002,-15.75));
#32741=CARTESIAN_POINT('Origin',(0.,9.00000000000002,0.));
#32742=CARTESIAN_POINT('Origin',(0.,9.00000000000002,0.));
#32743=CARTESIAN_POINT('',(-1.92881870865708E-15,0.,15.75));
#32744=CARTESIAN_POINT('Origin',(-14.25,8.5,0.));
#32745=CARTESIAN_POINT('',(-1.86758636869971E-15,8.5,-15.25));
#32746=CARTESIAN_POINT('Origin',(0.,8.5,0.));
#32747=CARTESIAN_POINT('',(-1.65327317884893E-15,8.5,13.5));
#32748=CARTESIAN_POINT('Origin',(0.,8.5,0.));
#32749=CARTESIAN_POINT('Origin',(0.,0.,0.));
#32750=CARTESIAN_POINT('',(0.,1.1015,13.5));
#32751=CARTESIAN_POINT('',(-1.65327317884893E-15,1.1015,-13.5));
#32752=CARTESIAN_POINT('Origin',(0.,1.1015,0.));
#32753=CARTESIAN_POINT('Origin',(0.,1.1015,0.));
#32754=CARTESIAN_POINT('',(-1.65327317884893E-15,0.,13.5));
#32755=CARTESIAN_POINT('Origin',(0.,8.5,0.));
#32756=CARTESIAN_POINT('',(-1.86758636869971E-15,8.5,-15.25));
#32757=CARTESIAN_POINT('Origin',(0.,0.,0.));
#32758=CARTESIAN_POINT('',(-1.51837833392285E-15,-2.7393655125078E-16,-12.3985));
#32759=CARTESIAN_POINT('',(-1.51837833392285E-15,0.,-12.3985));
#32760=CARTESIAN_POINT('Origin',(0.,0.,0.));
#32761=CARTESIAN_POINT('Origin',(0.,10.,0.));
#32762=CARTESIAN_POINT('',(-1.10218211923262E-15,10.,9.));
#32763=CARTESIAN_POINT('Origin',(0.,10.,0.));
#32764=CARTESIAN_POINT('Origin',(0.,10.,0.));
#32765=CARTESIAN_POINT('',(0.,1.00000000000001,9.));
#32766=CARTESIAN_POINT('',(-1.10218211923262E-15,10.,9.));
#32767=CARTESIAN_POINT('Origin',(0.,1.00000000000001,0.));
#32768=CARTESIAN_POINT('Origin',(0.,1.00000000000001,0.));
#32769=CARTESIAN_POINT('',(0.,-8.72560844392489E-16,10.));
#32770=CARTESIAN_POINT('',(-1.10218211923262E-15,1.00000000000001,9.));
#32771=CARTESIAN_POINT('Origin',(0.,-8.72560844392489E-16,0.));
#32772=CARTESIAN_POINT('Origin',(0.,-8.72560844392489E-16,0.));
#32773=CARTESIAN_POINT('',(0.,0.,0.));
#32774=CARTESIAN_POINT('Origin',(0.,1.92592994438724E-31,0.));
#32775=CARTESIAN_POINT('',(-1.43712301879942E-15,1.60428730688303E-16,-11.735));
#32776=CARTESIAN_POINT('Origin',(-1.59755174948772E-15,1.92592994438724E-31,
-13.045));
#32777=CARTESIAN_POINT('Origin',(0.,-1.60428730688303E-16,0.));
#32778=CARTESIAN_POINT('',(0.,0.,0.));
#32779=CARTESIAN_POINT('Origin',(0.,-3.25,0.));
#32780=CARTESIAN_POINT('',(-3.48274395975477,-3.25,5.49479033678217));
#32781=CARTESIAN_POINT('',(-3.01725604024523,-3.25,5.76353991241553));
#32782=CARTESIAN_POINT('',(-6.5,-3.25,3.75277674973257));
#32783=CARTESIAN_POINT('',(-6.5,-3.25,0.268749575633325));
#32784=CARTESIAN_POINT('Origin',(0.,-3.25,0.));
#32785=CARTESIAN_POINT('',(-6.5,-3.25,-0.268749575633324));
#32786=CARTESIAN_POINT('',(-6.5,-3.25,-3.75277674973257));
#32787=CARTESIAN_POINT('',(-3.48274395975469,-3.25,-5.49479033678222));
#32788=CARTESIAN_POINT('Origin',(0.,-3.25,0.));
#32789=CARTESIAN_POINT('',(-3.01725604024531,-3.25,-5.76353991241548));
#32790=CARTESIAN_POINT('',(-2.05562859610134E-16,-3.25,-7.50555349946514));
#32791=CARTESIAN_POINT('',(3.01725604024528,-3.25,-5.7635399124155));
#32792=CARTESIAN_POINT('Origin',(0.,-3.25,0.));
#32793=CARTESIAN_POINT('',(3.48274395975473,-3.25,-5.4947903367822));
#32794=CARTESIAN_POINT('',(6.5,-3.25,-3.75277674973257));
#32795=CARTESIAN_POINT('',(6.5,-3.25,-0.26874957563335));
#32796=CARTESIAN_POINT('Origin',(0.,-3.25,0.));
#32797=CARTESIAN_POINT('',(6.5,-3.25,0.268749575633349));
#32798=CARTESIAN_POINT('',(6.5,-3.25,3.75277674973257));
#32799=CARTESIAN_POINT('',(3.48274395975475,-3.25,5.49479033678219));
#32800=CARTESIAN_POINT('Origin',(0.,-3.25,0.));
#32801=CARTESIAN_POINT('',(3.01725604024525,-3.25,5.76353991241551));
#32802=CARTESIAN_POINT('',(-5.5631874730702E-16,-3.25,7.50555349946513));
#32803=CARTESIAN_POINT('Origin',(0.,-3.25,0.));
#32804=CARTESIAN_POINT('',(0.0048323552597593,-3.25,3.49158803373809));
#32805=CARTESIAN_POINT('Origin',(0.00483235525975973,-3.25,-0.00841196626190816));
#32806=CARTESIAN_POINT('Origin',(0.,3.25,0.));
#32807=CARTESIAN_POINT('',(-3.48274395975477,3.25,5.49479033678217));
#32808=CARTESIAN_POINT('',(-6.5,3.25,0.268749575633325));
#32809=CARTESIAN_POINT('Origin',(0.,3.25,0.));
#32810=CARTESIAN_POINT('',(-3.01725604024523,3.25,5.76353991241552));
#32811=CARTESIAN_POINT('',(-6.5,3.25,3.75277674973257));
#32812=CARTESIAN_POINT('',(3.01725604024525,3.25,5.76353991241551));
#32813=CARTESIAN_POINT('Origin',(0.,3.25,0.));
#32814=CARTESIAN_POINT('',(3.48274395975475,3.25,5.49479033678219));
#32815=CARTESIAN_POINT('',(-5.5631874730702E-16,3.25,7.50555349946513));
#32816=CARTESIAN_POINT('',(6.5,3.25,0.268749575633349));
#32817=CARTESIAN_POINT('Origin',(0.,3.25,0.));
#32818=CARTESIAN_POINT('',(6.5,3.25,-0.26874957563335));
#32819=CARTESIAN_POINT('',(6.5,3.25,3.75277674973257));
#32820=CARTESIAN_POINT('',(3.48274395975473,3.25,-5.4947903367822));
#32821=CARTESIAN_POINT('Origin',(0.,3.25,0.));
#32822=CARTESIAN_POINT('',(3.01725604024528,3.25,-5.7635399124155));
#32823=CARTESIAN_POINT('',(6.5,3.25,-3.75277674973257));
#32824=CARTESIAN_POINT('',(-3.01725604024531,3.25,-5.76353991241549));
#32825=CARTESIAN_POINT('Origin',(0.,3.25,0.));
#32826=CARTESIAN_POINT('',(-3.48274395975469,3.25,-5.49479033678222));
#32827=CARTESIAN_POINT('',(-2.05562859610134E-16,3.25,-7.50555349946514));
#32828=CARTESIAN_POINT('',(-6.5,3.25,-0.268749575633324));
#32829=CARTESIAN_POINT('Origin',(0.,3.25,0.));
#32830=CARTESIAN_POINT('',(-6.5,3.25,-3.75277674973257));
#32831=CARTESIAN_POINT('',(0.00483235525975973,3.25,3.49158803373809));
#32832=CARTESIAN_POINT('Origin',(0.00483235525975973,3.25,-0.00841196626190816));
#32833=CARTESIAN_POINT('Origin',(6.5,3.25,3.75277674973257));
#32834=CARTESIAN_POINT('',(6.5,2.25,3.75277674973257));
#32835=CARTESIAN_POINT('',(6.5,-2.25,3.75277674973257));
#32836=CARTESIAN_POINT('',(6.5,3.25,3.75277674973257));
#32837=CARTESIAN_POINT('Ctrl Pts',(6.5,-2.25000000000019,3.75277674973218));
#32838=CARTESIAN_POINT('Ctrl Pts',(6.5,-3.18317224509129,1.88643225954984));
#32839=CARTESIAN_POINT('Ctrl Pts',(6.5,-3.25000000000011,0.268749575630723));
#32840=CARTESIAN_POINT('',(6.5,-2.25,-3.75277674973257));
#32841=CARTESIAN_POINT('Ctrl Pts',(6.5,-3.25000000000011,-0.268749575630739));
#32842=CARTESIAN_POINT('Ctrl Pts',(6.5,-3.18317224509129,-1.88643225954986));
#32843=CARTESIAN_POINT('Ctrl Pts',(6.5,-2.25000000000019,-3.7527767497322));
#32844=CARTESIAN_POINT('',(6.5,2.25,-3.75277674973257));
#32845=CARTESIAN_POINT('',(6.5,3.25,-3.75277674973257));
#32846=CARTESIAN_POINT('Ctrl Pts',(6.5,2.25000000000018,-3.75277674973221));
#32847=CARTESIAN_POINT('Ctrl Pts',(6.5,3.18317224509129,-1.88643225954986));
#32848=CARTESIAN_POINT('Ctrl Pts',(6.5,3.25000000000011,-0.268749575630731));
#32849=CARTESIAN_POINT('Ctrl Pts',(6.5,3.25000000000011,0.268749575630733));
#32850=CARTESIAN_POINT('Ctrl Pts',(6.5,3.18317224509129,1.88643225954985));
#32851=CARTESIAN_POINT('Ctrl Pts',(6.5,2.25000000000019,3.75277674973219));
#32852=CARTESIAN_POINT('Origin',(6.5,3.25,-3.75277674973257));
#32853=CARTESIAN_POINT('Ctrl Pts',(6.49999999999967,-2.25000000000019,-3.75277674973276));
#32854=CARTESIAN_POINT('Ctrl Pts',(4.88369825928862,-3.18317224509131,-4.68594899482394));
#32855=CARTESIAN_POINT('Ctrl Pts',(3.48274395975245,-3.25000000000011,-5.49479033678352));
#32856=CARTESIAN_POINT('',(-1.73472347597681E-15,-2.25,-7.50555349946514));
#32857=CARTESIAN_POINT('Ctrl Pts',(3.01725604024755,-3.25000000000011,-5.76353991241419));
#32858=CARTESIAN_POINT('Ctrl Pts',(1.61630174071138,-3.1831722450913,-6.57238125437376));
#32859=CARTESIAN_POINT('Ctrl Pts',(3.27578534860098E-13,-2.25000000000019,
-7.50555349946495));
#32860=CARTESIAN_POINT('',(-1.73472347597681E-15,2.25,-7.50555349946514));
#32861=CARTESIAN_POINT('',(-2.05562859610134E-16,3.25,-7.50555349946514));
#32862=CARTESIAN_POINT('Ctrl Pts',(3.28190693931138E-13,2.25000000000019,
-7.50555349946495));
#32863=CARTESIAN_POINT('Ctrl Pts',(1.61630174071138,3.1831722450913,-6.57238125437376));
#32864=CARTESIAN_POINT('Ctrl Pts',(3.01725604024755,3.25000000000011,-5.76353991241419));
#32865=CARTESIAN_POINT('Ctrl Pts',(3.48274395975246,3.25000000000011,-5.49479033678351));
#32866=CARTESIAN_POINT('Ctrl Pts',(4.88369825928863,3.1831722450913,-4.68594899482394));
#32867=CARTESIAN_POINT('Ctrl Pts',(6.49999999999968,2.25000000000019,-3.75277674973275));
#32868=CARTESIAN_POINT('Origin',(-2.05562859610134E-16,3.25,-7.50555349946514));
#32869=CARTESIAN_POINT('Ctrl Pts',(-3.25455340652671E-13,-2.25000000000019,
-7.50555349946495));
#32870=CARTESIAN_POINT('Ctrl Pts',(-1.61630174071139,-3.18317224509132,
-6.57238125437375));
#32871=CARTESIAN_POINT('Ctrl Pts',(-3.01725604024758,-3.25000000000011,
-5.76353991241417));
#32872=CARTESIAN_POINT('',(-6.5,-2.25,-3.75277674973257));
#32873=CARTESIAN_POINT('Ctrl Pts',(-3.48274395975242,-3.25000000000011,
-5.49479033678353));
#32874=CARTESIAN_POINT('Ctrl Pts',(-4.88369825928861,-3.18317224509131,
-4.68594899482395));
#32875=CARTESIAN_POINT('Ctrl Pts',(-6.49999999999967,-2.25000000000019,
-3.75277674973276));
#32876=CARTESIAN_POINT('',(-6.5,2.25,-3.75277674973257));
#32877=CARTESIAN_POINT('',(-6.5,3.25,-3.75277674973257));
#32878=CARTESIAN_POINT('Ctrl Pts',(-6.49999999999968,2.25000000000018,-3.75277674973276));
#32879=CARTESIAN_POINT('Ctrl Pts',(-4.88369825928861,3.18317224509131,-4.68594899482395));
#32880=CARTESIAN_POINT('Ctrl Pts',(-3.48274395975242,3.25000000000011,-5.49479033678354));
#32881=CARTESIAN_POINT('Ctrl Pts',(-3.01725604024757,3.25000000000011,-5.76353991241418));
#32882=CARTESIAN_POINT('Ctrl Pts',(-1.61630174071139,3.18317224509131,-6.57238125437376));
#32883=CARTESIAN_POINT('Ctrl Pts',(-3.28190693931137E-13,2.25000000000019,
-7.50555349946495));
#32884=CARTESIAN_POINT('Origin',(-6.5,3.25,-3.75277674973257));
#32885=CARTESIAN_POINT('Ctrl Pts',(-6.5,-2.25000000000018,-3.7527767497322));
#32886=CARTESIAN_POINT('Ctrl Pts',(-6.5,-3.1831722450913,-1.88643225954984));
#32887=CARTESIAN_POINT('Ctrl Pts',(-6.5,-3.25000000000011,-0.268749575630697));
#32888=CARTESIAN_POINT('',(-6.5,-2.25,3.75277674973256));
#32889=CARTESIAN_POINT('Ctrl Pts',(-6.5,-3.25000000000011,0.268749575630706));
#32890=CARTESIAN_POINT('Ctrl Pts',(-6.5,-3.1831722450913,1.88643225954984));
#32891=CARTESIAN_POINT('Ctrl Pts',(-6.5,-2.25000000000019,3.75277674973219));
#32892=CARTESIAN_POINT('',(-6.5,2.25,3.75277674973256));
#32893=CARTESIAN_POINT('',(-6.5,3.25,3.75277674973257));
#32894=CARTESIAN_POINT('Ctrl Pts',(-6.5,2.25000000000019,3.75277674973219));
#32895=CARTESIAN_POINT('Ctrl Pts',(-6.5,3.1831722450913,1.88643225954984));
#32896=CARTESIAN_POINT('Ctrl Pts',(-6.5,3.25000000000011,0.268749575630717));
#32897=CARTESIAN_POINT('Ctrl Pts',(-6.5,3.25000000000011,-0.268749575630705));
#32898=CARTESIAN_POINT('Ctrl Pts',(-6.5,3.1831722450913,-1.88643225954984));
#32899=CARTESIAN_POINT('Ctrl Pts',(-6.5,2.25000000000019,-3.75277674973219));
#32900=CARTESIAN_POINT('Origin',(-6.5,3.25,3.75277674973257));
#32901=CARTESIAN_POINT('Ctrl Pts',(-6.49999999999968,-2.25000000000019,
3.75277674973275));
#32902=CARTESIAN_POINT('Ctrl Pts',(-4.88369825928865,-3.18317224509129,
4.68594899482393));
#32903=CARTESIAN_POINT('Ctrl Pts',(-3.4827439597525,-3.25000000000011,5.49479033678349));
#32904=CARTESIAN_POINT('',(-3.03576608295941E-15,-2.25,7.50555349946514));
#32905=CARTESIAN_POINT('Ctrl Pts',(-3.0172560402475,-3.25000000000011,5.76353991241422));
#32906=CARTESIAN_POINT('Ctrl Pts',(-1.61630174071135,-3.18317224509129,
6.57238125437378));
#32907=CARTESIAN_POINT('Ctrl Pts',(-3.26061967569079E-13,-2.25000000000019,
7.50555349946495));
#32908=CARTESIAN_POINT('',(-3.03576608295941E-15,2.25,7.50555349946514));
#32909=CARTESIAN_POINT('',(-5.5631874730702E-16,3.25,7.50555349946513));
#32910=CARTESIAN_POINT('Ctrl Pts',(-3.3274047249765E-13,2.25000000000019,
7.50555349946494));
#32911=CARTESIAN_POINT('Ctrl Pts',(-1.61630174071135,3.18317224509129,6.57238125437378));
#32912=CARTESIAN_POINT('Ctrl Pts',(-3.0172560402475,3.25000000000011,5.76353991241422));
#32913=CARTESIAN_POINT('Ctrl Pts',(-3.48274395975249,3.25000000000011,5.49479033678349));
#32914=CARTESIAN_POINT('Ctrl Pts',(-4.88369825928865,3.1831722450913,4.68594899482393));
#32915=CARTESIAN_POINT('Ctrl Pts',(-6.49999999999968,2.25000000000019,3.75277674973275));
#32916=CARTESIAN_POINT('Origin',(-5.5631874730702E-16,3.25,7.50555349946513));
#32917=CARTESIAN_POINT('Ctrl Pts',(3.2697190794369E-13,-2.25000000000019,
7.50555349946494));
#32918=CARTESIAN_POINT('Ctrl Pts',(1.61630174071137,-3.1831722450913,6.57238125437376));
#32919=CARTESIAN_POINT('Ctrl Pts',(3.01725604024753,-3.25000000000011,5.7635399124142));
#32920=CARTESIAN_POINT('Ctrl Pts',(3.48274395975248,-3.25000000000011,5.49479033678349));
#32921=CARTESIAN_POINT('Ctrl Pts',(4.88369825928864,-3.1831722450913,4.68594899482393));
#32922=CARTESIAN_POINT('Ctrl Pts',(6.49999999999968,-2.25000000000019,3.75277674973275));
#32923=CARTESIAN_POINT('Ctrl Pts',(6.49999999999967,2.25000000000019,3.75277674973275));
#32924=CARTESIAN_POINT('Ctrl Pts',(4.88369825928864,3.1831722450913,4.68594899482393));
#32925=CARTESIAN_POINT('Ctrl Pts',(3.48274395975247,3.25000000000011,5.4947903367835));
#32926=CARTESIAN_POINT('Ctrl Pts',(3.01725604024752,3.25000000000011,5.7635399124142));
#32927=CARTESIAN_POINT('Ctrl Pts',(1.61630174071136,3.1831722450913,6.57238125437377));
#32928=CARTESIAN_POINT('Ctrl Pts',(3.19394455369212E-13,2.25000000000019,
7.50555349946495));
#32929=CARTESIAN_POINT('Origin',(0.,3.25,0.));
#32930=CARTESIAN_POINT('Origin',(0.,3.25,0.));
#32931=CARTESIAN_POINT('Origin',(0.,3.25,0.));
#32932=CARTESIAN_POINT('Origin',(0.,3.25,0.));
#32933=CARTESIAN_POINT('Origin',(0.,3.25,0.));
#32934=CARTESIAN_POINT('Origin',(0.,3.25,0.));
#32935=CARTESIAN_POINT('Origin',(0.,-3.25,0.));
#32936=CARTESIAN_POINT('Origin',(0.,-3.25,0.));
#32937=CARTESIAN_POINT('Origin',(0.,-3.25,0.));
#32938=CARTESIAN_POINT('Origin',(0.,-3.25,0.));
#32939=CARTESIAN_POINT('Origin',(0.,-3.25,0.));
#32940=CARTESIAN_POINT('Origin',(0.,-3.25,0.));
#32941=CARTESIAN_POINT('Origin',(0.00483235525975973,-3.25,-0.00841196626190816));
#32942=CARTESIAN_POINT('',(0.0048323552597593,-3.25,3.49158803373809));
#32943=CARTESIAN_POINT('',(0.,0.,0.));
#32944=CARTESIAN_POINT('',(0.,-13.75,0.));
#32945=CARTESIAN_POINT('',(-3.50552920025393E-15,6.71103657744647E-32,-63.15));
#32946=CARTESIAN_POINT('',(7.70371977754894E-31,1.18553248860419E-12,-339.55));
#32947=CARTESIAN_POINT('',(-4.14945855453653E-15,-13.9,-74.75));
#32948=CARTESIAN_POINT('',(9.42828894462855E-15,-7.46329069311107E-17,-405.05));
#32949=CARTESIAN_POINT('',(0.00483235525976916,0.00841196626190809,-366.8));
#32950=CARTESIAN_POINT('',(9.4282889446288E-15,-7.46329069311107E-17,-396.55));
#32951=CARTESIAN_POINT('',(5.50340067261495E-13,0.,-402.697619766708));
#32952=CARTESIAN_POINT('',(-0.00483235525976768,-0.0084119662619122,-375.3));
#32953=UNCERTAINTY_MEASURE_WITH_UNIT(LENGTH_MEASURE(0.01),#33017,
'DISTANCE_ACCURACY_VALUE',
'Maximum model space distance between geometric entities at asserted c
onnectivities');
#32954=UNCERTAINTY_MEASURE_WITH_UNIT(LENGTH_MEASURE(0.01),#33017,
'DISTANCE_ACCURACY_VALUE',
'Maximum model space distance between geometric entities at asserted c
onnectivities');
#32955=UNCERTAINTY_MEASURE_WITH_UNIT(LENGTH_MEASURE(0.01),#33017,
'DISTANCE_ACCURACY_VALUE',
'Maximum model space distance between geometric entities at asserted c
onnectivities');
#32956=UNCERTAINTY_MEASURE_WITH_UNIT(LENGTH_MEASURE(0.01),#33017,
'DISTANCE_ACCURACY_VALUE',
'Maximum model space distance between geometric entities at asserted c
onnectivities');
#32957=UNCERTAINTY_MEASURE_WITH_UNIT(LENGTH_MEASURE(0.01),#33017,
'DISTANCE_ACCURACY_VALUE',
'Maximum model space distance between geometric entities at asserted c
onnectivities');
#32958=UNCERTAINTY_MEASURE_WITH_UNIT(LENGTH_MEASURE(0.01),#33017,
'DISTANCE_ACCURACY_VALUE',
'Maximum model space distance between geometric entities at asserted c
onnectivities');
#32959=UNCERTAINTY_MEASURE_WITH_UNIT(LENGTH_MEASURE(0.01),#33017,
'DISTANCE_ACCURACY_VALUE',
'Maximum model space distance between geometric entities at asserted c
onnectivities');
#32960=UNCERTAINTY_MEASURE_WITH_UNIT(LENGTH_MEASURE(0.01),#33017,
'DISTANCE_ACCURACY_VALUE',
'Maximum model space distance between geometric entities at asserted c
onnectivities');
#32961=UNCERTAINTY_MEASURE_WITH_UNIT(LENGTH_MEASURE(0.01),#33017,
'DISTANCE_ACCURACY_VALUE',
'Maximum model space distance between geometric entities at asserted c
onnectivities');
#32962=UNCERTAINTY_MEASURE_WITH_UNIT(LENGTH_MEASURE(0.01),#33017,
'DISTANCE_ACCURACY_VALUE',
'Maximum model space distance between geometric entities at asserted c
onnectivities');
#32963=UNCERTAINTY_MEASURE_WITH_UNIT(LENGTH_MEASURE(0.01),#33017,
'DISTANCE_ACCURACY_VALUE',
'Maximum model space distance between geometric entities at asserted c
onnectivities');
#32964=UNCERTAINTY_MEASURE_WITH_UNIT(LENGTH_MEASURE(0.01),#33017,
'DISTANCE_ACCURACY_VALUE',
'Maximum model space distance between geometric entities at asserted c
onnectivities');
#32965=UNCERTAINTY_MEASURE_WITH_UNIT(LENGTH_MEASURE(0.01),#33017,
'DISTANCE_ACCURACY_VALUE',
'Maximum model space distance between geometric entities at asserted c
onnectivities');
#32966=UNCERTAINTY_MEASURE_WITH_UNIT(LENGTH_MEASURE(0.01),#33017,
'DISTANCE_ACCURACY_VALUE',
'Maximum model space distance between geometric entities at asserted c
onnectivities');
#32967=UNCERTAINTY_MEASURE_WITH_UNIT(LENGTH_MEASURE(0.01),#33017,
'DISTANCE_ACCURACY_VALUE',
'Maximum model space distance between geometric entities at asserted c
onnectivities');
#32968=UNCERTAINTY_MEASURE_WITH_UNIT(LENGTH_MEASURE(0.01),#33017,
'DISTANCE_ACCURACY_VALUE',
'Maximum model space distance between geometric entities at asserted c
onnectivities');
#32969=UNCERTAINTY_MEASURE_WITH_UNIT(LENGTH_MEASURE(0.01),#33017,
'DISTANCE_ACCURACY_VALUE',
'Maximum model space distance between geometric entities at asserted c
onnectivities');
#32970=UNCERTAINTY_MEASURE_WITH_UNIT(LENGTH_MEASURE(0.01),#33017,
'DISTANCE_ACCURACY_VALUE',
'Maximum model space distance between geometric entities at asserted c
onnectivities');
#32971=UNCERTAINTY_MEASURE_WITH_UNIT(LENGTH_MEASURE(0.01),#33017,
'DISTANCE_ACCURACY_VALUE',
'Maximum model space distance between geometric entities at asserted c
onnectivities');
#32972=UNCERTAINTY_MEASURE_WITH_UNIT(LENGTH_MEASURE(0.01),#33017,
'DISTANCE_ACCURACY_VALUE',
'Maximum model space distance between geometric entities at asserted c
onnectivities');
#32973=UNCERTAINTY_MEASURE_WITH_UNIT(LENGTH_MEASURE(0.01),#33017,
'DISTANCE_ACCURACY_VALUE',
'Maximum model space distance between geometric entities at asserted c
onnectivities');
#32974=UNCERTAINTY_MEASURE_WITH_UNIT(LENGTH_MEASURE(0.01),#33017,
'DISTANCE_ACCURACY_VALUE',
'Maximum model space distance between geometric entities at asserted c
onnectivities');
#32975=UNCERTAINTY_MEASURE_WITH_UNIT(LENGTH_MEASURE(0.01),#33017,
'DISTANCE_ACCURACY_VALUE',
'Maximum model space distance between geometric entities at asserted c
onnectivities');
#32976=UNCERTAINTY_MEASURE_WITH_UNIT(LENGTH_MEASURE(0.01),#33017,
'DISTANCE_ACCURACY_VALUE',
'Maximum model space distance between geometric entities at asserted c
onnectivities');
#32977=UNCERTAINTY_MEASURE_WITH_UNIT(LENGTH_MEASURE(0.01),#33017,
'DISTANCE_ACCURACY_VALUE',
'Maximum model space distance between geometric entities at asserted c
onnectivities');
#32978=UNCERTAINTY_MEASURE_WITH_UNIT(LENGTH_MEASURE(0.01),#33017,
'DISTANCE_ACCURACY_VALUE',
'Maximum model space distance between geometric entities at asserted c
onnectivities');
#32979=UNCERTAINTY_MEASURE_WITH_UNIT(LENGTH_MEASURE(0.01),#33017,
'DISTANCE_ACCURACY_VALUE',
'Maximum model space distance between geometric entities at asserted c
onnectivities');
#32980=UNCERTAINTY_MEASURE_WITH_UNIT(LENGTH_MEASURE(0.01),#33017,
'DISTANCE_ACCURACY_VALUE',
'Maximum model space distance between geometric entities at asserted c
onnectivities');
#32981=UNCERTAINTY_MEASURE_WITH_UNIT(LENGTH_MEASURE(0.01),#33017,
'DISTANCE_ACCURACY_VALUE',
'Maximum model space distance between geometric entities at asserted c
onnectivities');
#32982=UNCERTAINTY_MEASURE_WITH_UNIT(LENGTH_MEASURE(0.01),#33017,
'DISTANCE_ACCURACY_VALUE',
'Maximum model space distance between geometric entities at asserted c
onnectivities');
#32983=UNCERTAINTY_MEASURE_WITH_UNIT(LENGTH_MEASURE(0.01),#33017,
'DISTANCE_ACCURACY_VALUE',
'Maximum model space distance between geometric entities at asserted c
onnectivities');
#32984=UNCERTAINTY_MEASURE_WITH_UNIT(LENGTH_MEASURE(0.01),#33017,
'DISTANCE_ACCURACY_VALUE',
'Maximum model space distance between geometric entities at asserted c
onnectivities');
#32985=(
GEOMETRIC_REPRESENTATION_CONTEXT(3)
GLOBAL_UNCERTAINTY_ASSIGNED_CONTEXT((#32953))
GLOBAL_UNIT_ASSIGNED_CONTEXT((#33017,#33019,#33020))
REPRESENTATION_CONTEXT('','3D')
);
#32986=(
GEOMETRIC_REPRESENTATION_CONTEXT(3)
GLOBAL_UNCERTAINTY_ASSIGNED_CONTEXT((#32954))
GLOBAL_UNIT_ASSIGNED_CONTEXT((#33017,#33019,#33020))
REPRESENTATION_CONTEXT('','3D')
);
#32987=(
GEOMETRIC_REPRESENTATION_CONTEXT(3)
GLOBAL_UNCERTAINTY_ASSIGNED_CONTEXT((#32955))
GLOBAL_UNIT_ASSIGNED_CONTEXT((#33017,#33019,#33020))
REPRESENTATION_CONTEXT('','3D')
);
#32988=(
GEOMETRIC_REPRESENTATION_CONTEXT(3)
GLOBAL_UNCERTAINTY_ASSIGNED_CONTEXT((#32956))
GLOBAL_UNIT_ASSIGNED_CONTEXT((#33017,#33019,#33020))
REPRESENTATION_CONTEXT('','3D')
);
#32989=(
GEOMETRIC_REPRESENTATION_CONTEXT(3)
GLOBAL_UNCERTAINTY_ASSIGNED_CONTEXT((#32957))
GLOBAL_UNIT_ASSIGNED_CONTEXT((#33017,#33019,#33020))
REPRESENTATION_CONTEXT('','3D')
);
#32990=(
GEOMETRIC_REPRESENTATION_CONTEXT(3)
GLOBAL_UNCERTAINTY_ASSIGNED_CONTEXT((#32958))
GLOBAL_UNIT_ASSIGNED_CONTEXT((#33017,#33019,#33020))
REPRESENTATION_CONTEXT('','3D')
);
#32991=(
GEOMETRIC_REPRESENTATION_CONTEXT(3)
GLOBAL_UNCERTAINTY_ASSIGNED_CONTEXT((#32959))
GLOBAL_UNIT_ASSIGNED_CONTEXT((#33017,#33019,#33020))
REPRESENTATION_CONTEXT('','3D')
);
#32992=(
GEOMETRIC_REPRESENTATION_CONTEXT(3)
GLOBAL_UNCERTAINTY_ASSIGNED_CONTEXT((#32960))
GLOBAL_UNIT_ASSIGNED_CONTEXT((#33017,#33019,#33020))
REPRESENTATION_CONTEXT('','3D')
);
#32993=(
GEOMETRIC_REPRESENTATION_CONTEXT(3)
GLOBAL_UNCERTAINTY_ASSIGNED_CONTEXT((#32961))
GLOBAL_UNIT_ASSIGNED_CONTEXT((#33017,#33019,#33020))
REPRESENTATION_CONTEXT('','3D')
);
#32994=(
GEOMETRIC_REPRESENTATION_CONTEXT(3)
GLOBAL_UNCERTAINTY_ASSIGNED_CONTEXT((#32962))
GLOBAL_UNIT_ASSIGNED_CONTEXT((#33017,#33019,#33020))
REPRESENTATION_CONTEXT('','3D')
);
#32995=(
GEOMETRIC_REPRESENTATION_CONTEXT(3)
GLOBAL_UNCERTAINTY_ASSIGNED_CONTEXT((#32963))
GLOBAL_UNIT_ASSIGNED_CONTEXT((#33017,#33019,#33020))
REPRESENTATION_CONTEXT('','3D')
);
#32996=(
GEOMETRIC_REPRESENTATION_CONTEXT(3)
GLOBAL_UNCERTAINTY_ASSIGNED_CONTEXT((#32964))
GLOBAL_UNIT_ASSIGNED_CONTEXT((#33017,#33019,#33020))
REPRESENTATION_CONTEXT('','3D')
);
#32997=(
GEOMETRIC_REPRESENTATION_CONTEXT(3)
GLOBAL_UNCERTAINTY_ASSIGNED_CONTEXT((#32965))
GLOBAL_UNIT_ASSIGNED_CONTEXT((#33017,#33019,#33020))
REPRESENTATION_CONTEXT('','3D')
);
#32998=(
GEOMETRIC_REPRESENTATION_CONTEXT(3)
GLOBAL_UNCERTAINTY_ASSIGNED_CONTEXT((#32966))
GLOBAL_UNIT_ASSIGNED_CONTEXT((#33017,#33019,#33020))
REPRESENTATION_CONTEXT('','3D')
);
#32999=(
GEOMETRIC_REPRESENTATION_CONTEXT(3)
GLOBAL_UNCERTAINTY_ASSIGNED_CONTEXT((#32967))
GLOBAL_UNIT_ASSIGNED_CONTEXT((#33017,#33019,#33020))
REPRESENTATION_CONTEXT('','3D')
);
#33000=(
GEOMETRIC_REPRESENTATION_CONTEXT(3)
GLOBAL_UNCERTAINTY_ASSIGNED_CONTEXT((#32968))
GLOBAL_UNIT_ASSIGNED_CONTEXT((#33017,#33019,#33020))
REPRESENTATION_CONTEXT('','3D')
);
#33001=(
GEOMETRIC_REPRESENTATION_CONTEXT(3)
GLOBAL_UNCERTAINTY_ASSIGNED_CONTEXT((#32969))
GLOBAL_UNIT_ASSIGNED_CONTEXT((#33017,#33019,#33020))
REPRESENTATION_CONTEXT('','3D')
);
#33002=(
GEOMETRIC_REPRESENTATION_CONTEXT(3)
GLOBAL_UNCERTAINTY_ASSIGNED_CONTEXT((#32970))
GLOBAL_UNIT_ASSIGNED_CONTEXT((#33017,#33019,#33020))
REPRESENTATION_CONTEXT('','3D')
);
#33003=(
GEOMETRIC_REPRESENTATION_CONTEXT(3)
GLOBAL_UNCERTAINTY_ASSIGNED_CONTEXT((#32971))
GLOBAL_UNIT_ASSIGNED_CONTEXT((#33017,#33019,#33020))
REPRESENTATION_CONTEXT('','3D')
);
#33004=(
GEOMETRIC_REPRESENTATION_CONTEXT(3)
GLOBAL_UNCERTAINTY_ASSIGNED_CONTEXT((#32972))
GLOBAL_UNIT_ASSIGNED_CONTEXT((#33017,#33019,#33020))
REPRESENTATION_CONTEXT('','3D')
);
#33005=(
GEOMETRIC_REPRESENTATION_CONTEXT(3)
GLOBAL_UNCERTAINTY_ASSIGNED_CONTEXT((#32973))
GLOBAL_UNIT_ASSIGNED_CONTEXT((#33017,#33019,#33020))
REPRESENTATION_CONTEXT('','3D')
);
#33006=(
GEOMETRIC_REPRESENTATION_CONTEXT(3)
GLOBAL_UNCERTAINTY_ASSIGNED_CONTEXT((#32974))
GLOBAL_UNIT_ASSIGNED_CONTEXT((#33017,#33019,#33020))
REPRESENTATION_CONTEXT('','3D')
);
#33007=(
GEOMETRIC_REPRESENTATION_CONTEXT(3)
GLOBAL_UNCERTAINTY_ASSIGNED_CONTEXT((#32975))
GLOBAL_UNIT_ASSIGNED_CONTEXT((#33017,#33019,#33020))
REPRESENTATION_CONTEXT('','3D')
);
#33008=(
GEOMETRIC_REPRESENTATION_CONTEXT(3)
GLOBAL_UNCERTAINTY_ASSIGNED_CONTEXT((#32976))
GLOBAL_UNIT_ASSIGNED_CONTEXT((#33017,#33019,#33020))
REPRESENTATION_CONTEXT('','3D')
);
#33009=(
GEOMETRIC_REPRESENTATION_CONTEXT(3)
GLOBAL_UNCERTAINTY_ASSIGNED_CONTEXT((#32977))
GLOBAL_UNIT_ASSIGNED_CONTEXT((#33017,#33019,#33020))
REPRESENTATION_CONTEXT('','3D')
);
#33010=(
GEOMETRIC_REPRESENTATION_CONTEXT(3)
GLOBAL_UNCERTAINTY_ASSIGNED_CONTEXT((#32978))
GLOBAL_UNIT_ASSIGNED_CONTEXT((#33017,#33019,#33020))
REPRESENTATION_CONTEXT('','3D')
);
#33011=(
GEOMETRIC_REPRESENTATION_CONTEXT(3)
GLOBAL_UNCERTAINTY_ASSIGNED_CONTEXT((#32979))
GLOBAL_UNIT_ASSIGNED_CONTEXT((#33017,#33019,#33020))
REPRESENTATION_CONTEXT('','3D')
);
#33012=(
GEOMETRIC_REPRESENTATION_CONTEXT(3)
GLOBAL_UNCERTAINTY_ASSIGNED_CONTEXT((#32980))
GLOBAL_UNIT_ASSIGNED_CONTEXT((#33017,#33019,#33020))
REPRESENTATION_CONTEXT('','3D')
);
#33013=(
GEOMETRIC_REPRESENTATION_CONTEXT(3)
GLOBAL_UNCERTAINTY_ASSIGNED_CONTEXT((#32981))
GLOBAL_UNIT_ASSIGNED_CONTEXT((#33017,#33019,#33020))
REPRESENTATION_CONTEXT('','3D')
);
#33014=(
GEOMETRIC_REPRESENTATION_CONTEXT(3)
GLOBAL_UNCERTAINTY_ASSIGNED_CONTEXT((#32982))
GLOBAL_UNIT_ASSIGNED_CONTEXT((#33017,#33019,#33020))
REPRESENTATION_CONTEXT('','3D')
);
#33015=(
GEOMETRIC_REPRESENTATION_CONTEXT(3)
GLOBAL_UNCERTAINTY_ASSIGNED_CONTEXT((#32983))
GLOBAL_UNIT_ASSIGNED_CONTEXT((#33017,#33019,#33020))
REPRESENTATION_CONTEXT('','3D')
);
#33016=(
GEOMETRIC_REPRESENTATION_CONTEXT(3)
GLOBAL_UNCERTAINTY_ASSIGNED_CONTEXT((#32984))
GLOBAL_UNIT_ASSIGNED_CONTEXT((#33017,#33019,#33020))
REPRESENTATION_CONTEXT('','3D')
);
#33017=(
LENGTH_UNIT()
NAMED_UNIT(*)
SI_UNIT(.MILLI.,.METRE.)
);
#33018=(
LENGTH_UNIT()
NAMED_UNIT(*)
SI_UNIT($,.METRE.)
);
#33019=(
NAMED_UNIT(*)
PLANE_ANGLE_UNIT()
SI_UNIT($,.RADIAN.)
);
#33020=(
NAMED_UNIT(*)
SI_UNIT($,.STERADIAN.)
SOLID_ANGLE_UNIT()
);
#33021=SHAPE_DEFINITION_REPRESENTATION(#33052,#33124);
#33022=SHAPE_DEFINITION_REPRESENTATION(#33053,#33125);
#33023=SHAPE_DEFINITION_REPRESENTATION(#33054,#33126);
#33024=SHAPE_DEFINITION_REPRESENTATION(#33055,#33127);
#33025=SHAPE_DEFINITION_REPRESENTATION(#33056,#33128);
#33026=SHAPE_DEFINITION_REPRESENTATION(#33057,#33129);
#33027=SHAPE_DEFINITION_REPRESENTATION(#33058,#33130);
#33028=SHAPE_DEFINITION_REPRESENTATION(#33059,#33131);
#33029=SHAPE_DEFINITION_REPRESENTATION(#33060,#33132);
#33030=SHAPE_DEFINITION_REPRESENTATION(#33061,#33133);
#33031=SHAPE_DEFINITION_REPRESENTATION(#33070,#33134);
#33032=SHAPE_DEFINITION_REPRESENTATION(#33071,#33135);
#33033=SHAPE_DEFINITION_REPRESENTATION(#33072,#33136);
#33034=SHAPE_DEFINITION_REPRESENTATION(#33073,#33137);
#33035=SHAPE_DEFINITION_REPRESENTATION(#33074,#33138);
#33036=SHAPE_DEFINITION_REPRESENTATION(#33075,#33139);
#33037=SHAPE_DEFINITION_REPRESENTATION(#33076,#33140);
#33038=SHAPE_DEFINITION_REPRESENTATION(#33077,#33141);
#33039=SHAPE_DEFINITION_REPRESENTATION(#33078,#33142);
#33040=SHAPE_DEFINITION_REPRESENTATION(#33079,#33143);
#33041=SHAPE_DEFINITION_REPRESENTATION(#33080,#33144);
#33042=SHAPE_DEFINITION_REPRESENTATION(#33095,#33145);
#33043=SHAPE_DEFINITION_REPRESENTATION(#33096,#33146);
#33044=SHAPE_DEFINITION_REPRESENTATION(#33097,#33147);
#33045=SHAPE_DEFINITION_REPRESENTATION(#33098,#33148);
#33046=SHAPE_DEFINITION_REPRESENTATION(#33099,#33149);
#33047=SHAPE_DEFINITION_REPRESENTATION(#33100,#33150);
#33048=SHAPE_DEFINITION_REPRESENTATION(#33101,#33151);
#33049=SHAPE_DEFINITION_REPRESENTATION(#33111,#33152);
#33050=SHAPE_DEFINITION_REPRESENTATION(#33112,#33153);
#33051=SHAPE_DEFINITION_REPRESENTATION(#33113,#33154);
#33052=PRODUCT_DEFINITION_SHAPE('',$,#33156);
#33053=PRODUCT_DEFINITION_SHAPE('',$,#33157);
#33054=PRODUCT_DEFINITION_SHAPE('',$,#33158);
#33055=PRODUCT_DEFINITION_SHAPE('',$,#33159);
#33056=PRODUCT_DEFINITION_SHAPE('',$,#33160);
#33057=PRODUCT_DEFINITION_SHAPE('',$,#33161);
#33058=PRODUCT_DEFINITION_SHAPE('',$,#33162);
#33059=PRODUCT_DEFINITION_SHAPE('',$,#33163);
#33060=PRODUCT_DEFINITION_SHAPE('',$,#33164);
#33061=PRODUCT_DEFINITION_SHAPE('',$,#33165);
#33062=PRODUCT_DEFINITION_SHAPE($,$,#136);
#33063=PRODUCT_DEFINITION_SHAPE($,$,#137);
#33064=PRODUCT_DEFINITION_SHAPE($,$,#138);
#33065=PRODUCT_DEFINITION_SHAPE($,$,#139);
#33066=PRODUCT_DEFINITION_SHAPE($,$,#140);
#33067=PRODUCT_DEFINITION_SHAPE($,$,#141);
#33068=PRODUCT_DEFINITION_SHAPE($,$,#142);
#33069=PRODUCT_DEFINITION_SHAPE($,$,#143);
#33070=PRODUCT_DEFINITION_SHAPE('',$,#33166);
#33071=PRODUCT_DEFINITION_SHAPE('',$,#33167);
#33072=PRODUCT_DEFINITION_SHAPE('',$,#33168);
#33073=PRODUCT_DEFINITION_SHAPE('',$,#33169);
#33074=PRODUCT_DEFINITION_SHAPE('',$,#33170);
#33075=PRODUCT_DEFINITION_SHAPE('',$,#33171);
#33076=PRODUCT_DEFINITION_SHAPE('',$,#33172);
#33077=PRODUCT_DEFINITION_SHAPE('',$,#33173);
#33078=PRODUCT_DEFINITION_SHAPE('',$,#33174);
#33079=PRODUCT_DEFINITION_SHAPE('',$,#33175);
#33080=PRODUCT_DEFINITION_SHAPE('',$,#33176);
#33081=PRODUCT_DEFINITION_SHAPE($,$,#144);
#33082=PRODUCT_DEFINITION_SHAPE($,$,#145);
#33083=PRODUCT_DEFINITION_SHAPE($,$,#146);
#33084=PRODUCT_DEFINITION_SHAPE($,$,#147);
#33085=PRODUCT_DEFINITION_SHAPE($,$,#148);
#33086=PRODUCT_DEFINITION_SHAPE($,$,#149);
#33087=PRODUCT_DEFINITION_SHAPE($,$,#150);
#33088=PRODUCT_DEFINITION_SHAPE($,$,#151);
#33089=PRODUCT_DEFINITION_SHAPE($,$,#152);
#33090=PRODUCT_DEFINITION_SHAPE($,$,#153);
#33091=PRODUCT_DEFINITION_SHAPE($,$,#154);
#33092=PRODUCT_DEFINITION_SHAPE($,$,#155);
#33093=PRODUCT_DEFINITION_SHAPE($,$,#156);
#33094=PRODUCT_DEFINITION_SHAPE($,$,#157);
#33095=PRODUCT_DEFINITION_SHAPE('',$,#33177);
#33096=PRODUCT_DEFINITION_SHAPE('',$,#33178);
#33097=PRODUCT_DEFINITION_SHAPE('',$,#33179);
#33098=PRODUCT_DEFINITION_SHAPE('',$,#33180);
#33099=PRODUCT_DEFINITION_SHAPE('',$,#33181);
#33100=PRODUCT_DEFINITION_SHAPE('',$,#33182);
#33101=PRODUCT_DEFINITION_SHAPE('',$,#33183);
#33102=PRODUCT_DEFINITION_SHAPE($,$,#158);
#33103=PRODUCT_DEFINITION_SHAPE($,$,#159);
#33104=PRODUCT_DEFINITION_SHAPE($,$,#160);
#33105=PRODUCT_DEFINITION_SHAPE($,$,#161);
#33106=PRODUCT_DEFINITION_SHAPE($,$,#162);
#33107=PRODUCT_DEFINITION_SHAPE($,$,#163);
#33108=PRODUCT_DEFINITION_SHAPE($,$,#164);
#33109=PRODUCT_DEFINITION_SHAPE($,$,#165);
#33110=PRODUCT_DEFINITION_SHAPE($,$,#166);
#33111=PRODUCT_DEFINITION_SHAPE('',$,#33184);
#33112=PRODUCT_DEFINITION_SHAPE('',$,#33185);
#33113=PRODUCT_DEFINITION_SHAPE('',$,#33186);
#33114=PRODUCT_DEFINITION_SHAPE($,$,#167);
#33115=PRODUCT_DEFINITION_SHAPE($,$,#168);
#33116=PRODUCT_DEFINITION_SHAPE($,$,#169);
#33117=PRODUCT_DEFINITION_SHAPE($,$,#170);
#33118=PRODUCT_DEFINITION_SHAPE($,$,#171);
#33119=PRODUCT_DEFINITION_SHAPE($,$,#172);
#33120=PRODUCT_DEFINITION_SHAPE($,$,#173);
#33121=PRODUCT_DEFINITION_SHAPE($,$,#174);
#33122=PRODUCT_DEFINITION_SHAPE($,$,#175);
#33123=PRODUCT_DEFINITION_SHAPE($,$,#176);
#33124=SHAPE_REPRESENTATION('',(#10267,#11223,#11224,#11225,#11226,#11227,
#11228,#11229,#11230,#11231,#11232),#32985);
#33125=SHAPE_REPRESENTATION('',(#10268),#32986);
#33126=SHAPE_REPRESENTATION('',(#10518,#10691,#10692,#10693,#10694,#10695,
#10696,#10697,#10698),#32987);
#33127=SHAPE_REPRESENTATION('',(#10519),#32988);
#33128=SHAPE_REPRESENTATION('',(#10580),#32989);
#33129=SHAPE_REPRESENTATION('',(#10615),#32990);
#33130=SHAPE_REPRESENTATION('',(#10626),#32991);
#33131=SHAPE_REPRESENTATION('',(#10666),#32992);
#33132=SHAPE_REPRESENTATION('',(#10677),#32993);
#33133=SHAPE_REPRESENTATION('',(#10688),#32994);
#33134=SHAPE_REPRESENTATION('',(#10699),#32995);
#33135=SHAPE_REPRESENTATION('',(#10703,#10890,#10891,#10892,#10893,#10894,
#10895,#10896,#10897,#10898,#10899,#10900,#10901,#10902,#10903),#32996);
#33136=SHAPE_REPRESENTATION('',(#10704),#32997);
#33137=SHAPE_REPRESENTATION('',(#10767),#32998);
#33138=SHAPE_REPRESENTATION('',(#10782),#32999);
#33139=SHAPE_REPRESENTATION('',(#10807),#33000);
#33140=SHAPE_REPRESENTATION('',(#10814),#33001);
#33141=SHAPE_REPRESENTATION('',(#10835),#33002);
#33142=SHAPE_REPRESENTATION('',(#10868),#33003);
#33143=SHAPE_REPRESENTATION('',(#10875),#33004);
#33144=SHAPE_REPRESENTATION('',(#10881),#33005);
#33145=SHAPE_REPRESENTATION('',(#10904),#33006);
#33146=SHAPE_REPRESENTATION('',(#10922,#11150,#11151,#11152,#11153,#11154,
#11155,#11156,#11157,#11158),#33007);
#33147=SHAPE_REPRESENTATION('',(#10923),#33008);
#33148=SHAPE_REPRESENTATION('',(#11059),#33009);
#33149=SHAPE_REPRESENTATION('',(#11102),#33010);
#33150=SHAPE_REPRESENTATION('',(#11113),#33011);
#33151=SHAPE_REPRESENTATION('',(#11147),#33012);
#33152=SHAPE_REPRESENTATION('',(#11159),#33013);
#33153=SHAPE_REPRESENTATION('',(#11183),#33014);
#33154=SHAPE_REPRESENTATION('',(#11187),#33015);
#33155=PRODUCT_DEFINITION_CONTEXT('part definition',#33250,'design');
#33156=PRODUCT_DEFINITION('MAS-618','MAS-618',#33187,#33155);
#33157=PRODUCT_DEFINITION(
'P_Torque Wrench_Handle_PRT-TQ-1012-01_M_Rev01','PRT-TQ-1012-01',#33188,
#33155);
#33158=PRODUCT_DEFINITION(
'S_Torque Wrench_Housing Mechanism_S_RH-1004_M_Rev01',
'S_Torque Wrench_Housing Mechanism_S_RH-1004_M_Rev01',#33189,#33155);
#33159=PRODUCT_DEFINITION(
'P_Torque Wrench_Housing_PRT-RH-1004-02_M_Rev01','PRT-RH-1004-02',#33190,
#33155);
#33160=PRODUCT_DEFINITION('P_Torque Wrench_Pawl_PRT-RH-1004-03_M_Rev00',
'PRT-RH-1004-03',#33191,#33155);
#33161=PRODUCT_DEFINITION(
'P_Torque Wrench_Pin_PRT-BL-RH-1004-05_M_Rev00','PRT-BL-RH-1004-05',#33192,
#33155);
#33162=PRODUCT_DEFINITION('P_Torque Wrench_Knob_PRT-RH-1004-04_M_Rev02',
'PRT-RH-1004-04',#33193,#33155);
#33163=PRODUCT_DEFINITION(
'BO21-002_Spring_PUR-HW-4007_0.7x5x6_M_Rev00 (C)','PUR-HW-4007',#33194,
#33155);
#33164=PRODUCT_DEFINITION(
'BO21-002_Spring_PUR-HW-4008_0.7x5x10_M_Rev00 (C)','PUR-HW-4008',#33195,
#33155);
#33165=PRODUCT_DEFINITION('BO21-001_Ball_PUR-BR-9003_M_Rev00',
'PUR-BR-9003',#33196,#33155);
#33166=PRODUCT_DEFINITION(
'BO26-002_O Ring_PUR-HW-4059_20.4 OD x 13.8 ID x 3.3 T','PUR-HW-4059',#33197,
#33155);
#33167=PRODUCT_DEFINITION(
'S_Torque Wrench_Barrel Assembly_S_Torque Wrench_Barrel Assembly_TQ-10
12_M_Rev01',
'S_Torque Wrench_Barrel Assembly_S_Torque Wrench_Barrel Assembly_TQ-10
12_M_Rev01',#33198,#33155);
#33168=PRODUCT_DEFINITION(
'P_Torque Wrench_Barrel_PRT-TQ-1012-02_M_Rev01','PRT-TQ-1012-02',#33199,
#33155);
#33169=PRODUCT_DEFINITION(
'P_Torque Wrench_Barrel Nut_PRT-TQ-1012-12_M_Rev01','PRT-TQ-1012-12',#33200,
#33155);
#33170=PRODUCT_DEFINITION(
'P_Torque Wrench_Calibration Screw_PRT-TQ1012-10_M_Rev00',
'PRT-TQ1012-10',#33201,#33155);
#33171=PRODUCT_DEFINITION(
'BO21-002_Spring_PUR-HW-4060_18.5T_4 mm x 18.6 mm x 100 mm (C)',
'PUR-HW-4060',#33202,#33155);
#33172=PRODUCT_DEFINITION(
'P_Torque Wrench_Plunger_PRT-TQ-1012-08_M_Rev01','PRT-TQ-1012-08',#33203,
#33155);
#33173=PRODUCT_DEFINITION(
'P_Torque Wrench_Pivot Cube_PRT-TQ-1012-07_M_Rev00','PRT-TQ-1012-07',#33204,
#33155);
#33174=PRODUCT_DEFINITION(
'P_Torque Wrench_External C-Clip_PUR-HW-4062_M_Rev00','PUR-HW-4062',#33205,
#33155);
#33175=PRODUCT_DEFINITION(
'P_Torque Wrench_Push Plate_PRT-TQ-1012-09_M_Rev00','PRT-TQ-1012-09',#33206,
#33155);
#33176=PRODUCT_DEFINITION('P_Torque Wrench_Push Bush_PRT-TQ-1020',
'PRT-TQ-1020',#33207,#33155);
#33177=PRODUCT_DEFINITION(
'P_Torque Wrench_Head Handle Lock Pin_PRT-TQ-1012-14_M_Rev00',
'PRT-TQ-1012-14',#33208,#33155);
#33178=PRODUCT_DEFINITION(
'S_Torque Wrench_Handle Grip Drive Assembly_S_Torque Wrench Handle Gri
p Drive Assembly-TQ-1012_M_Rev01',
'S_Torque Wrench_Handle Grip Drive Assembly_S_Torque Wrench Handle Gri
p Drive Assembly-TQ-1012_M_Rev01',#33209,#33155);
#33179=PRODUCT_DEFINITION(
'P_Torque Wrench_Hand Grip_PRT-TQ-1012-03_M_Rev01','PRT-TQ-1012-03',#33210,
#33155);
#33180=PRODUCT_DEFINITION(
'P_Torque Wrench_Handle Grip Drive_PRT-TQ-1012-11_M_Rev00',
'PRT-TQ-1012-11',#33211,#33155);
#33181=PRODUCT_DEFINITION(
'BO21-002_Spring_PUR-HW-4061_4T_1.2 mm x 29.5 mm x 28 mm (C)',
'PUR-HW-4061',#33212,#33155);
#33182=PRODUCT_DEFINITION(
'P_Torque Wrench_Locking Ring_PRT-TQ-1012-05_M_Rev00','PRT-TQ-1012-04',
#33213,#33155);
#33183=PRODUCT_DEFINITION('BO21-001_Ball_D3.5 Steel Ball',
'BO21-001_Ball_D3.5 Steel Ball',#33214,#33155);
#33184=PRODUCT_DEFINITION(
'P_Torque Wrench_End Cap_PRT-TQ-1012-05_M_Rev00','PRT-TQ-1012-05',#33215,
#33155);
#33185=PRODUCT_DEFINITION('BO26-002_O Ring_End Cap O-ring',
'BO26-002_O Ring_End Cap O-ring',#33216,#33155);
#33186=PRODUCT_DEFINITION('P_Torque Wrench_Handle Grip Drive Nut_1012',
'P_Torque Wrench_Handle Grip Drive Nut_1012',#33217,#33155);
#33187=PRODUCT_DEFINITION_FORMATION('',$,#33252);
#33188=PRODUCT_DEFINITION_FORMATION('',$,#33253);
#33189=PRODUCT_DEFINITION_FORMATION('',$,#33254);
#33190=PRODUCT_DEFINITION_FORMATION('',$,#33255);
#33191=PRODUCT_DEFINITION_FORMATION('',$,#33256);
#33192=PRODUCT_DEFINITION_FORMATION('',$,#33257);
#33193=PRODUCT_DEFINITION_FORMATION('',$,#33258);
#33194=PRODUCT_DEFINITION_FORMATION('',$,#33259);
#33195=PRODUCT_DEFINITION_FORMATION('',$,#33260);
#33196=PRODUCT_DEFINITION_FORMATION('',$,#33261);
#33197=PRODUCT_DEFINITION_FORMATION('',$,#33262);
#33198=PRODUCT_DEFINITION_FORMATION('',$,#33263);
#33199=PRODUCT_DEFINITION_FORMATION('',$,#33264);
#33200=PRODUCT_DEFINITION_FORMATION('',$,#33265);
#33201=PRODUCT_DEFINITION_FORMATION('',$,#33266);
#33202=PRODUCT_DEFINITION_FORMATION('',$,#33267);
#33203=PRODUCT_DEFINITION_FORMATION('',$,#33268);
#33204=PRODUCT_DEFINITION_FORMATION('',$,#33269);
#33205=PRODUCT_DEFINITION_FORMATION('',$,#33270);
#33206=PRODUCT_DEFINITION_FORMATION('',$,#33271);
#33207=PRODUCT_DEFINITION_FORMATION('',$,#33272);
#33208=PRODUCT_DEFINITION_FORMATION('',$,#33273);
#33209=PRODUCT_DEFINITION_FORMATION('',$,#33274);
#33210=PRODUCT_DEFINITION_FORMATION('',$,#33275);
#33211=PRODUCT_DEFINITION_FORMATION('',$,#33276);
#33212=PRODUCT_DEFINITION_FORMATION('',$,#33277);
#33213=PRODUCT_DEFINITION_FORMATION('',$,#33278);
#33214=PRODUCT_DEFINITION_FORMATION('',$,#33279);
#33215=PRODUCT_DEFINITION_FORMATION('',$,#33280);
#33216=PRODUCT_DEFINITION_FORMATION('',$,#33281);
#33217=PRODUCT_DEFINITION_FORMATION('',$,#33282);
#33218=PRODUCT_RELATED_PRODUCT_CATEGORY('MAS-618',
'MAS-618',(#33252));
#33219=PRODUCT_RELATED_PRODUCT_CATEGORY('PRT-TQ-1012-01',
'PRT-TQ-1012-01',(#33253));
#33220=PRODUCT_RELATED_PRODUCT_CATEGORY(
'S_Torque Wrench_Housing Mechanism_S_RH-1004_M_Rev01',
'S_Torque Wrench_Housing Mechanism_S_RH-1004_M_Rev01',(#33254));
#33221=PRODUCT_RELATED_PRODUCT_CATEGORY('PRT-RH-1004-02',
'PRT-RH-1004-02',(#33255));
#33222=PRODUCT_RELATED_PRODUCT_CATEGORY('PRT-RH-1004-03',
'PRT-RH-1004-03',(#33256));
#33223=PRODUCT_RELATED_PRODUCT_CATEGORY('PRT-BL-RH-1004-05',
'PRT-BL-RH-1004-05',(#33257));
#33224=PRODUCT_RELATED_PRODUCT_CATEGORY('PRT-RH-1004-04',
'PRT-RH-1004-04',(#33258));
#33225=PRODUCT_RELATED_PRODUCT_CATEGORY('PUR-HW-4007','PUR-HW-4007',(#33259));
#33226=PRODUCT_RELATED_PRODUCT_CATEGORY('PUR-HW-4008','PUR-HW-4008',(#33260));
#33227=PRODUCT_RELATED_PRODUCT_CATEGORY('PUR-BR-9003','PUR-BR-9003',(#33261));
#33228=PRODUCT_RELATED_PRODUCT_CATEGORY('PUR-HW-4059','PUR-HW-4059',(#33262));
#33229=PRODUCT_RELATED_PRODUCT_CATEGORY(
'S_Torque Wrench_Barrel Assembly_S_Torque Wrench_Barrel Assembly_TQ-10
12_M_Rev01',
'S_Torque Wrench_Barrel Assembly_S_Torque Wrench_Barrel Assembly_TQ-10
12_M_Rev01',(#33263));
#33230=PRODUCT_RELATED_PRODUCT_CATEGORY('PRT-TQ-1012-02',
'PRT-TQ-1012-02',(#33264));
#33231=PRODUCT_RELATED_PRODUCT_CATEGORY('PRT-TQ-1012-12',
'PRT-TQ-1012-12',(#33265));
#33232=PRODUCT_RELATED_PRODUCT_CATEGORY('PRT-TQ1012-10','PRT-TQ1012-10',
(#33266));
#33233=PRODUCT_RELATED_PRODUCT_CATEGORY('PUR-HW-4060','PUR-HW-4060',(#33267));
#33234=PRODUCT_RELATED_PRODUCT_CATEGORY('PRT-TQ-1012-08',
'PRT-TQ-1012-08',(#33268));
#33235=PRODUCT_RELATED_PRODUCT_CATEGORY('PRT-TQ-1012-07',
'PRT-TQ-1012-07',(#33269));
#33236=PRODUCT_RELATED_PRODUCT_CATEGORY('PUR-HW-4062','PUR-HW-4062',(#33270));
#33237=PRODUCT_RELATED_PRODUCT_CATEGORY('PRT-TQ-1012-09',
'PRT-TQ-1012-09',(#33271));
#33238=PRODUCT_RELATED_PRODUCT_CATEGORY('PRT-TQ-1020','PRT-TQ-1020',(#33272));
#33239=PRODUCT_RELATED_PRODUCT_CATEGORY('PRT-TQ-1012-14',
'PRT-TQ-1012-14',(#33273));
#33240=PRODUCT_RELATED_PRODUCT_CATEGORY(
'S_Torque Wrench_Handle Grip Drive Assembly_S_Torque Wrench Handle Gri
p Drive Assembly-TQ-1012_M_Rev01',
'S_Torque Wrench_Handle Grip Drive Assembly_S_Torque Wrench Handle Gri
p Drive Assembly-TQ-1012_M_Rev01',(#33274));
#33241=PRODUCT_RELATED_PRODUCT_CATEGORY('PRT-TQ-1012-03',
'PRT-TQ-1012-03',(#33275));
#33242=PRODUCT_RELATED_PRODUCT_CATEGORY('PRT-TQ-1012-11',
'PRT-TQ-1012-11',(#33276));
#33243=PRODUCT_RELATED_PRODUCT_CATEGORY('PUR-HW-4061','PUR-HW-4061',(#33277));
#33244=PRODUCT_RELATED_PRODUCT_CATEGORY('PRT-TQ-1012-04',
'PRT-TQ-1012-04',(#33278));
#33245=PRODUCT_RELATED_PRODUCT_CATEGORY('BO21-001_Ball_D3.5 Steel Ball',
'BO21-001_Ball_D3.5 Steel Ball',(#33279));
#33246=PRODUCT_RELATED_PRODUCT_CATEGORY('PRT-TQ-1012-05',
'PRT-TQ-1012-05',(#33280));
#33247=PRODUCT_RELATED_PRODUCT_CATEGORY(
'BO26-002_O Ring_End Cap O-ring','BO26-002_O Ring_End Cap O-ring',(#33281));
#33248=PRODUCT_RELATED_PRODUCT_CATEGORY(
'P_Torque Wrench_Handle Grip Drive Nut_1012',
'P_Torque Wrench_Handle Grip Drive Nut_1012',(#33282));
#33249=APPLICATION_PROTOCOL_DEFINITION('international standard',
'automotive_design',2009,#33250);
#33250=APPLICATION_CONTEXT(
'Core Data for Automotive Mechanical Design Process');
#33251=PRODUCT_CONTEXT('part definition',#33250,'mechanical');
#33252=PRODUCT('MAS-618','MAS-618','STEP AP214',(#33251));
#33253=PRODUCT('P_Torque Wrench_Handle_PRT-TQ-1012-01_M_Rev01',
'PRT-TQ-1012-01',$,(#33251));
#33254=PRODUCT('S_Torque Wrench_Housing Mechanism_S_RH-1004_M_Rev01',
'S_Torque Wrench_Housing Mechanism_S_RH-1004_M_Rev01',$,(#33251));
#33255=PRODUCT('P_Torque Wrench_Housing_PRT-RH-1004-02_M_Rev01',
'PRT-RH-1004-02',$,(#33251));
#33256=PRODUCT('P_Torque Wrench_Pawl_PRT-RH-1004-03_M_Rev00',
'PRT-RH-1004-03',$,(#33251));
#33257=PRODUCT('P_Torque Wrench_Pin_PRT-BL-RH-1004-05_M_Rev00',
'PRT-BL-RH-1004-05',$,(#33251));
#33258=PRODUCT('P_Torque Wrench_Knob_PRT-RH-1004-04_M_Rev02',
'PRT-RH-1004-04',$,(#33251));
#33259=PRODUCT('BO21-002_Spring_PUR-HW-4007_0.7x5x6_M_Rev00 (C)',
'PUR-HW-4007',$,(#33251));
#33260=PRODUCT('BO21-002_Spring_PUR-HW-4008_0.7x5x10_M_Rev00 (C)',
'PUR-HW-4008',$,(#33251));
#33261=PRODUCT('BO21-001_Ball_PUR-BR-9003_M_Rev00','PUR-BR-9003',$,(#33251));
#33262=PRODUCT('BO26-002_O Ring_PUR-HW-4059_20.4 OD x 13.8 ID x 3.3 T',
'PUR-HW-4059',$,(#33251));
#33263=PRODUCT(
'S_Torque Wrench_Barrel Assembly_S_Torque Wrench_Barrel Assembly_TQ-10
12_M_Rev01',
'S_Torque Wrench_Barrel Assembly_S_Torque Wrench_Barrel Assembly_TQ-10
12_M_Rev01',$,(#33251));
#33264=PRODUCT('P_Torque Wrench_Barrel_PRT-TQ-1012-02_M_Rev01',
'PRT-TQ-1012-02',$,(#33251));
#33265=PRODUCT('P_Torque Wrench_Barrel Nut_PRT-TQ-1012-12_M_Rev01',
'PRT-TQ-1012-12',$,(#33251));
#33266=PRODUCT(
'P_Torque Wrench_Calibration Screw_PRT-TQ1012-10_M_Rev00',
'PRT-TQ1012-10',$,(#33251));
#33267=PRODUCT(
'BO21-002_Spring_PUR-HW-4060_18.5T_4 mm x 18.6 mm x 100 mm (C)',
'PUR-HW-4060',$,(#33251));
#33268=PRODUCT('P_Torque Wrench_Plunger_PRT-TQ-1012-08_M_Rev01',
'PRT-TQ-1012-08',$,(#33251));
#33269=PRODUCT('P_Torque Wrench_Pivot Cube_PRT-TQ-1012-07_M_Rev00',
'PRT-TQ-1012-07',$,(#33251));
#33270=PRODUCT('P_Torque Wrench_External C-Clip_PUR-HW-4062_M_Rev00',
'PUR-HW-4062',$,(#33251));
#33271=PRODUCT('P_Torque Wrench_Push Plate_PRT-TQ-1012-09_M_Rev00',
'PRT-TQ-1012-09',$,(#33251));
#33272=PRODUCT('P_Torque Wrench_Push Bush_PRT-TQ-1020','PRT-TQ-1020',$,
(#33251));
#33273=PRODUCT(
'P_Torque Wrench_Head Handle Lock Pin_PRT-TQ-1012-14_M_Rev00',
'PRT-TQ-1012-14',$,(#33251));
#33274=PRODUCT(
'S_Torque Wrench_Handle Grip Drive Assembly_S_Torque Wrench Handle Gri
p Drive Assembly-TQ-1012_M_Rev01',
'S_Torque Wrench_Handle Grip Drive Assembly_S_Torque Wrench Handle Gri
p Drive Assembly-TQ-1012_M_Rev01',$,(#33251));
#33275=PRODUCT('P_Torque Wrench_Hand Grip_PRT-TQ-1012-03_M_Rev01',
'PRT-TQ-1012-03',$,(#33251));
#33276=PRODUCT(
'P_Torque Wrench_Handle Grip Drive_PRT-TQ-1012-11_M_Rev00',
'PRT-TQ-1012-11',$,(#33251));
#33277=PRODUCT(
'BO21-002_Spring_PUR-HW-4061_4T_1.2 mm x 29.5 mm x 28 mm (C)',
'PUR-HW-4061',$,(#33251));
#33278=PRODUCT('P_Torque Wrench_Locking Ring_PRT-TQ-1012-05_M_Rev00',
'PRT-TQ-1012-04',$,(#33251));
#33279=PRODUCT('BO21-001_Ball_D3.5 Steel Ball',
'BO21-001_Ball_D3.5 Steel Ball',$,(#33251));
#33280=PRODUCT('P_Torque Wrench_End Cap_PRT-TQ-1012-05_M_Rev00',
'PRT-TQ-1012-05',$,(#33251));
#33281=PRODUCT('BO26-002_O Ring_End Cap O-ring',
'BO26-002_O Ring_End Cap O-ring',$,(#33251));
#33282=PRODUCT('P_Torque Wrench_Handle Grip Drive Nut_1012',
'P_Torque Wrench_Handle Grip Drive Nut_1012',$,(#33251));
#33283=PRESENTATION_STYLE_ASSIGNMENT((#33290));
#33284=PRESENTATION_STYLE_ASSIGNMENT((#33291));
#33285=PRESENTATION_STYLE_ASSIGNMENT((#33292));
#33286=PRESENTATION_STYLE_ASSIGNMENT((#33293));
#33287=PRESENTATION_STYLE_ASSIGNMENT((#33294));
#33288=PRESENTATION_STYLE_ASSIGNMENT((#33295));
#33289=PRESENTATION_STYLE_ASSIGNMENT((#33296));
#33290=SURFACE_STYLE_USAGE(.BOTH.,#33297);
#33291=SURFACE_STYLE_USAGE(.BOTH.,#33298);
#33292=SURFACE_STYLE_USAGE(.BOTH.,#33299);
#33293=SURFACE_STYLE_USAGE(.BOTH.,#33300);
#33294=SURFACE_STYLE_USAGE(.BOTH.,#33301);
#33295=SURFACE_STYLE_USAGE(.BOTH.,#33302);
#33296=SURFACE_STYLE_USAGE(.BOTH.,#33303);
#33297=SURFACE_SIDE_STYLE('',(#33304));
#33298=SURFACE_SIDE_STYLE('',(#33305));
#33299=SURFACE_SIDE_STYLE('',(#33306));
#33300=SURFACE_SIDE_STYLE('',(#33307));
#33301=SURFACE_SIDE_STYLE('',(#33308));
#33302=SURFACE_SIDE_STYLE('',(#33309));
#33303=SURFACE_SIDE_STYLE('',(#33310));
#33304=SURFACE_STYLE_FILL_AREA(#33311);
#33305=SURFACE_STYLE_FILL_AREA(#33312);
#33306=SURFACE_STYLE_FILL_AREA(#33313);
#33307=SURFACE_STYLE_FILL_AREA(#33314);
#33308=SURFACE_STYLE_FILL_AREA(#33315);
#33309=SURFACE_STYLE_FILL_AREA(#33316);
#33310=SURFACE_STYLE_FILL_AREA(#33317);
#33311=FILL_AREA_STYLE('Steel - Satin',(#33318));
#33312=FILL_AREA_STYLE('Opaque(186,91,6)',(#33319));
#33313=FILL_AREA_STYLE('Opaque(202,209,238)',(#33320));
#33314=FILL_AREA_STYLE('Opaque(178,178,178)',(#33321));
#33315=FILL_AREA_STYLE('Opaque(76,76,76)',(#33322));
#33316=FILL_AREA_STYLE('Opaque(192,192,192)',(#33323));
#33317=FILL_AREA_STYLE('Opaque(255,255,255)',(#33324));
#33318=FILL_AREA_STYLE_COLOUR('Steel - Satin',#33325);
#33319=FILL_AREA_STYLE_COLOUR('Opaque(186,91,6)',#33326);
#33320=FILL_AREA_STYLE_COLOUR('Opaque(202,209,238)',#33327);
#33321=FILL_AREA_STYLE_COLOUR('Opaque(178,178,178)',#33328);
#33322=FILL_AREA_STYLE_COLOUR('Opaque(76,76,76)',#33329);
#33323=FILL_AREA_STYLE_COLOUR('Opaque(192,192,192)',#33330);
#33324=FILL_AREA_STYLE_COLOUR('Opaque(255,255,255)',#33331);
#33325=COLOUR_RGB('Steel - Satin', 0.09019608, 0.27058824, 0.51372549);
#33326=COLOUR_RGB('Opaque(186,91,6)', 0.09019608, 0.27058824, 0.51372549);
#33327=COLOUR_RGB('Opaque(202,209,238)', 0.08235294, 0.09019608, 0.10196078);
#33328=COLOUR_RGB('Opaque(178,178,178)', 0.66274510, 0.83137255, 0.94901961);
#33329=COLOUR_RGB('Opaque(76,76,76)', 0.31764706, 0.68627451, 0.89019608);
#33330=COLOUR_RGB('Opaque(192,192,192)', 0.72549020, 0.75294118, 0.79215686);
#33331=COLOUR_RGB('Opaque(255,255,255)', 0.08235294, 0.09019608, 0.10196078);
ENDSEC;
END-ISO-10303-21;
